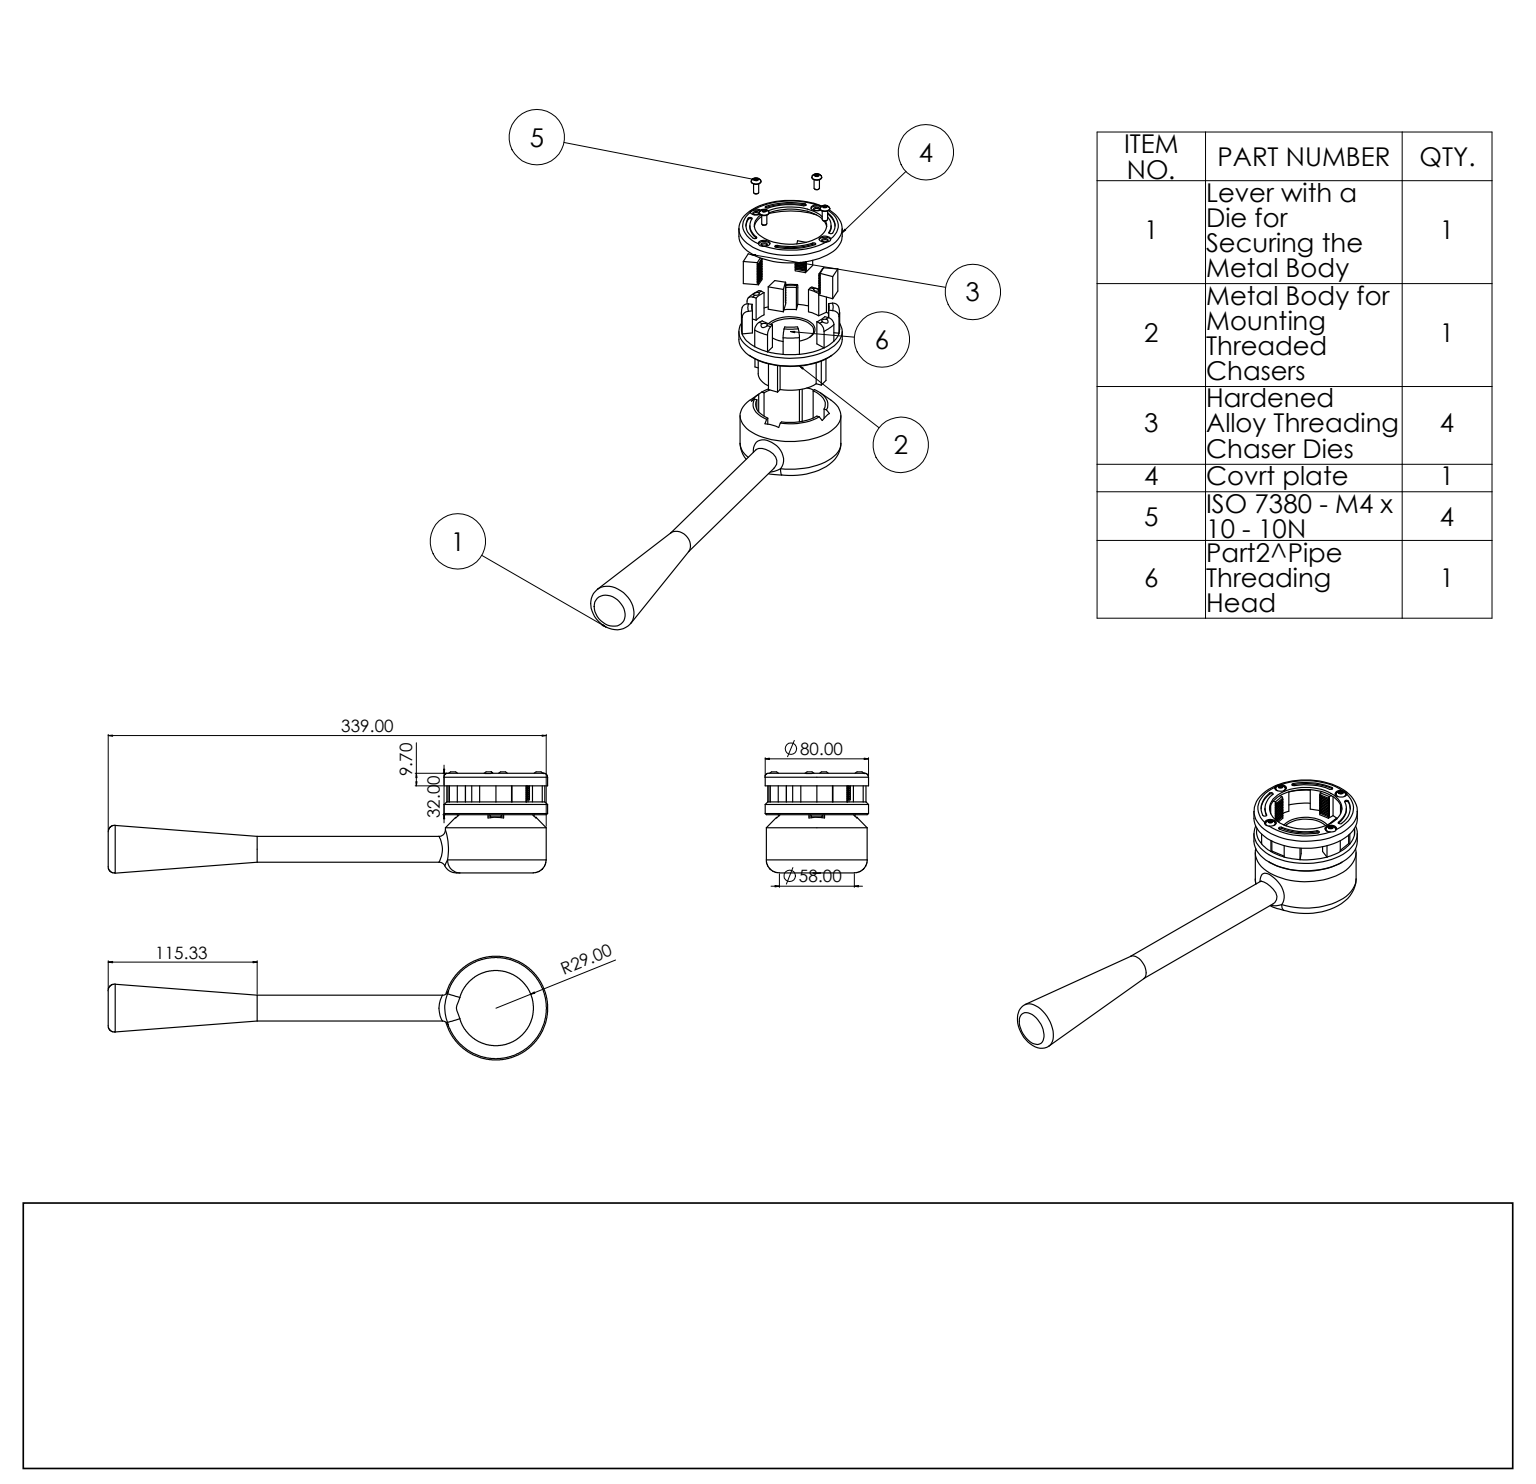
ISO-10303-21;
HEADER;
FILE_DESCRIPTION (('STEP AP214'),
    '1' );
FILE_NAME ('MAS-312',
    '2026-10-19T14:05:14',
    ( '' ),
    ( '' ),
    'SwSTEP 2.0',
    'SolidWorks 2025',
    '' );
FILE_SCHEMA (( 'AUTOMOTIVE_DESIGN' ));
ENDSEC;

DATA;
#1 = AXIS2_PLACEMENT_3D ( 'NONE', #3987, #6980, #243 ) ;
#2 = CARTESIAN_POINT ( 'NONE',  ( -12.48950176432141923, 54.99999999999999289, -35.88888888888889284 ) ) ;
#3 = ORIENTED_EDGE ( 'NONE', *, *, #1774, .T. ) ;
#4 = DIRECTION ( 'NONE',  ( 1.000000000000000000, 0.000000000000000000, -0.000000000000000000 ) ) ;
#5 = CARTESIAN_POINT ( 'NONE',  ( 3.853297297556091738, -8.887944228554063741, 39.26446342091823993 ) ) ;
#6 = ORIENTED_EDGE ( 'NONE', *, *, #748, .T. ) ;
#7 = DIRECTION ( 'NONE',  ( 0.000000000000000000, 0.000000000000000000, 1.000000000000000000 ) ) ;
#8 = LINE ( 'NONE', #7609, #8604 ) ;
#9 = ORIENTED_EDGE ( 'NONE', *, *, #8476, .T. ) ;
#10 = CARTESIAN_POINT ( 'NONE',  ( 11.49838106938660509, -4.251877780921969219, 37.26706069643609709 ) ) ;
#11 = ITEM_DEFINED_TRANSFORMATION ( 'NONE', 'NONE', #6463,  #6314 ) ;
#12 = ORIENTED_EDGE ( 'NONE', *, *, #8842, .T. ) ;
#13 = CARTESIAN_POINT ( 'NONE',  ( 6.000000000000007994, -10.00000000000000533, 31.00000000000000711 ) ) ;
#14 = CARTESIAN_POINT ( 'NONE',  ( 6.000000000000007994, 28.28385863652523824, 30.12488991936162108 ) ) ;
#15 = ORIENTED_EDGE ( 'NONE', *, *, #6125, .T. ) ;
#16 = CARTESIAN_POINT ( 'NONE',  ( 0.000000000000000000, 39.99999999999999289, 0.000000000000000000 ) ) ;
#17 = ORIENTED_EDGE ( 'NONE', *, *, #1471, .T. ) ;
#18 = CARTESIAN_POINT ( 'NONE',  ( 1.030449557444946671E-26, 53.50000000000031264, -26.00000000000004974 ) ) ;
#19 = DIRECTION ( 'NONE',  ( 0.000000000000000000, 0.000000000000000000, 1.000000000000000000 ) ) ;
#20 = CARTESIAN_POINT ( 'NONE',  ( -0.01963426291156584666, -6.705128248126137613, 43.99999014335539016 ) ) ;
#21 = MECHANICAL_DESIGN_GEOMETRIC_PRESENTATION_REPRESENTATION (  '', ( #1599 ), #7104 ) ;
#22 = VERTEX_POINT ( 'NONE', #2863 ) ;
#23 = CARTESIAN_POINT ( 'NONE',  ( -7.995545880304240960, 59.98659813632739457, 32.45264704635820152 ) ) ;
#24 = ORIENTED_EDGE ( 'NONE', *, *, #464, .F. ) ;
#25 = PRODUCT_DEFINITION_CONTEXT ( 'detailed design', #5808, 'design' ) ;
#26 = ORIENTED_EDGE ( 'NONE', *, *, #454, .F. ) ;
#28 = AXIS2_PLACEMENT_3D ( 'NONE', #4537, #730, #2939 ) ;
#27 = PLANE ( 'NONE',  #7404 ) ;
#29 = CARTESIAN_POINT ( 'NONE',  ( -0.01628753085184865904, -6.705134819200520901, 38.99999783451422530 ) ) ;
#30 = FACE_OUTER_BOUND ( 'NONE', #6374, .T. ) ;
#31 = DIRECTION ( 'NONE',  ( 0.000000000000000000, 0.000000000000000000, 1.000000000000000000 ) ) ;
#32 = ORIENTED_EDGE ( 'NONE', *, *, #3378, .T. ) ;
#33 = CARTESIAN_POINT ( 'NONE',  ( 28.34870838944214100, 59.99999999999999289, 9.815840903884559765 ) ) ;
#34 = ADVANCED_FACE ( 'NONE', ( #5878 ), #8015, .T. ) ;
#35 = EDGE_CURVE ( 'NONE', #8414, #7328, #2773, .T. ) ;
#36 = ORIENTED_EDGE ( 'NONE', *, *, #1808, .T. ) ;
#37 = CARTESIAN_POINT ( 'NONE',  ( -7.819489076939736272, 61.89591950820473443, 36.97167050927867393 ) ) ;
#38 = CARTESIAN_POINT ( 'NONE',  ( 1.084683744678891232E-26, 59.63872771225970837, -25.64778813235487220 ) ) ;
#39 = VECTOR ( 'NONE', #8891, 1000.000000000000000 ) ;
#40 = CARTESIAN_POINT ( 'NONE',  ( -8.673617379884032514E-16, 30.00000000000000000, -4.000000000000002665 ) ) ;
#41 = EDGE_CURVE ( 'NONE', #3849, #2645, #7411, .T. ) ;
#42 = CARTESIAN_POINT ( 'NONE',  ( 1.300000000000000044, -0.7216878364870317197, -1.250000000000000000 ) ) ;
#43 = CYLINDRICAL_SURFACE ( 'NONE', #4602, 1.999999999999999556 ) ;
#44 = DIRECTION ( 'NONE',  ( -1.000000000000000000, 0.000000000000000000, 0.000000000000000000 ) ) ;
#45 = ORIENTED_EDGE ( 'NONE', *, *, #2688, .T. ) ;
#46 = DIRECTION ( 'NONE',  ( -0.000000000000000000, 0.000000000000000000, 1.000000000000000000 ) ) ;
#47 = VECTOR ( 'NONE', #1280, 1000.000000000000000 ) ;
#48 = ADVANCED_FACE ( 'NONE', ( #1481 ), #9105, .T. ) ;
#49 = VERTEX_POINT ( 'NONE', #7520 ) ;
#50 = DIRECTION ( 'NONE',  ( 0.000000000000000000, 0.000000000000000000, 1.000000000000000000 ) ) ;
#51 = EDGE_CURVE ( 'NONE', #326, #7682, #6952, .T. ) ;
#52 = ORIENTED_EDGE ( 'NONE', *, *, #3525, .F. ) ;
#53 = CARTESIAN_POINT ( 'NONE',  ( 38.00000000000000711, 59.99999999999999289, 1.288922537256478387E-13 ) ) ;
#54 = CARTESIAN_POINT ( 'NONE',  ( 4.579605370182076030, -8.646111723837565322, 39.15306555959272572 ) ) ;
#55 = CIRCLE ( 'NONE', #3026, 27.00000000000000355 ) ;
#56 = CIRCLE ( 'NONE', #3832, 38.00000000000000711 ) ;
#57 = EDGE_LOOP ( 'NONE', ( #2932, #7865, #7571, #5966, #8095 ) ) ;
#58 = DIRECTION ( 'NONE',  ( 0.000000000000000000, 1.000000000000000000, 0.000000000000000000 ) ) ;
#59 = DIRECTION ( 'NONE',  ( -1.000000000000000000, 0.000000000000000000, 1.084202172485503448E-16 ) ) ;
#60 = ORIENTED_EDGE ( 'NONE', *, *, #1877, .F. ) ;
#61 = AXIS2_PLACEMENT_3D ( 'NONE', #6025, #2270, #8317 ) ;
#62 = CARTESIAN_POINT ( 'NONE',  ( 10.00081333311621989, 3.643253863043277363, 37.85858479645732899 ) ) ;
#63 = PRODUCT_CONTEXT ( 'NONE', #3923, 'mechanical' ) ;
#64 = VERTEX_POINT ( 'NONE', #213 ) ;
#65 = EDGE_LOOP ( 'NONE', ( #1698, #9286, #7170, #5423 ) ) ;
#66 = LINE ( 'NONE', #799, #8451 ) ;
#67 = CARTESIAN_POINT ( 'NONE',  ( -26.32489316217636954, -15.00000000000000000, 6.000000000000009770 ) ) ;
#68 = CARTESIAN_POINT ( 'NONE',  ( -3.999999999999999112, 28.99999999999997158, 24.67792535850613334 ) ) ;
#69 = ORIENTED_EDGE ( 'NONE', *, *, #3277, .T. ) ;
#70 = CARTESIAN_POINT ( 'NONE',  ( 0.000000000000000000, 0.000000000000000000, 0.000000000000000000 ) ) ;
#71 = VERTEX_POINT ( 'NONE', #9199 ) ;
#72 = CARTESIAN_POINT ( 'NONE',  ( -9.983292374582678264, 3.962892183205132479, 41.37334990339741125 ) ) ;
#73 = DIRECTION ( 'NONE',  ( 0.000000000000000000, 1.000000000000000000, 0.000000000000000000 ) ) ;
#74 = EDGE_CURVE ( 'NONE', #2204, #4788, #7083, .T. ) ;
#75 = DIRECTION ( 'NONE',  ( -1.735493991486225972E-29, 6.508102468073347395E-30, 1.000000000000000000 ) ) ;
#76 = AXIS2_PLACEMENT_3D ( 'NONE', #8734, #591, #7241 ) ;
#77 = VERTEX_POINT ( 'NONE', #3810 ) ;
#78 = CARTESIAN_POINT ( 'NONE',  ( 28.33333333333337478, 39.99999999999999289, -9.860132971832594961 ) ) ;
#79 = CARTESIAN_POINT ( 'NONE',  ( 20.99999999999999645, 30.00000000000000000, 4.000000000000000888 ) ) ;
#80 = ORIENTED_EDGE ( 'NONE', *, *, #3650, .T. ) ;
#81 = EDGE_LOOP ( 'NONE', ( #9222, #5342, #9321, #2491 ) ) ;
#82 = CARTESIAN_POINT ( 'NONE',  ( -2.771370799027269349, -6.331017003992445602, 38.93346330084214202 ) ) ;
#83 = CARTESIAN_POINT ( 'NONE',  ( 0.000000000000000000, 0.000000000000000000, 0.000000000000000000 ) ) ;
#84 = AXIS2_PLACEMENT_3D ( 'NONE', #4346, #782, #3690 ) ;
#85 = AXIS2_PLACEMENT_3D ( 'NONE', #944, #4059, #1772 ) ;
#86 = DIRECTION ( 'NONE',  ( 0.000000000000000000, 0.000000000000000000, 1.000000000000000000 ) ) ;
#87 = PRODUCT_DEFINITION_SHAPE ( 'NONE', 'NONE',  #9761 ) ;
#88 = ORIENTED_EDGE ( 'NONE', *, *, #8502, .F. ) ;
#89 = CARTESIAN_POINT ( 'NONE',  ( 5.562309845534588959, 60.99999999999999289, -30.56426808735054479 ) ) ;
#90 = AXIS2_PLACEMENT_3D ( 'NONE', #5171, #7481, #672 ) ;
#91 = ORIENTED_EDGE ( 'NONE', *, *, #7636, .T. ) ;
#92 = CARTESIAN_POINT ( 'NONE',  ( 5.562309845534588959, 49.99999999999999289, -33.06426808735054124 ) ) ;
#93 = EDGE_CURVE ( 'NONE', #9341, #7266, #8353, .T. ) ;
#94 = DIRECTION ( 'NONE',  ( -0.000000000000000000, -0.5000000000000001110, -0.8660254037844385966 ) ) ;
#95 = CARTESIAN_POINT ( 'NONE',  ( 24.67792535850613334, 0.000000000000000000, 4.000000000000000888 ) ) ;
#96 = CARTESIAN_POINT ( 'NONE',  ( 0.000000000000000000, 0.000000000000000000, 0.000000000000000000 ) ) ;
#97 = CARTESIAN_POINT ( 'NONE',  ( -6.850714361783683870, -15.00000000000000000, 28.25199985127544977 ) ) ;
#98 = CARTESIAN_POINT ( 'NONE',  ( -34.07933880998930221, 60.99999999999999289, 5.371095444502539173 ) ) ;
#99 = DIRECTION ( 'NONE',  ( 0.9449569463147374782, 0.000000000000000000, 0.3271946967961527619 ) ) ;
#100 = ORIENTED_EDGE ( 'NONE', *, *, #2687, .F. ) ;
#101 = DIRECTION ( 'NONE',  ( 0.000000000000000000, -1.000000000000000000, 0.000000000000000000 ) ) ;
#102 = VECTOR ( 'NONE', #2807, 1000.000000000000000 ) ;
#103 = VECTOR ( 'NONE', #6274, 1000.000000000000341 ) ;
#104 = CIRCLE ( 'NONE', #7815, 26.00000000000012790 ) ;
#105 = AXIS2_PLACEMENT_3D ( 'NONE', #139, #1748, #4771 ) ;
#106 = EDGE_CURVE ( 'NONE', #1933, #8061, #806, .T. ) ;
#107 = EDGE_CURVE ( 'NONE', #2537, #9428, #3759, .T. ) ;
#108 = VECTOR ( 'NONE', #4796, 1000.000000000000000 ) ;
#109 = AXIS2_PLACEMENT_3D ( 'NONE', #9198, #4705, #305 ) ;
#110 = CARTESIAN_POINT ( 'NONE',  ( 8.948640893600852668E-27, 42.50000000000020606, -25.00000000000000000 ) ) ;
#111 = ORIENTED_EDGE ( 'NONE', *, *, #684, .T. ) ;
#112 = DIRECTION ( 'NONE',  ( 0.000000000000000000, -1.000000000000000000, 0.000000000000000000 ) ) ;
#113 = CARTESIAN_POINT ( 'NONE',  ( 2.825938509006990174, -14.99999999999936762, 36.77312956257851084 ) ) ;
#114 = ORIENTED_EDGE ( 'NONE', *, *, #8852, .F. ) ;
#115 = ADVANCED_FACE ( 'NONE', ( #5243 ), #6016, .F. ) ;
#116 = DIRECTION ( 'NONE',  ( -0.000000000000000000, -1.000000000000000000, -0.000000000000000000 ) ) ;
#117 = AXIS2_PLACEMENT_3D ( 'NONE', #7294, #7143, #4982 ) ;
#118 = ADVANCED_FACE ( 'NONE', ( #1539 ), #6120, .T. ) ;
#119 = CARTESIAN_POINT ( 'NONE',  ( -8.216777476527294510, 42.50000000000020606, -23.61111111111107519 ) ) ;
#120 = CLOSED_SHELL ( 'NONE', ( #1419, #7952, #2099, #3958, #3679, #8907, #3700, #3725, #1256, #288, #9736, #7646, #7332, #6776, #8180, #48, #7507, #2171, #4864, #7401, #2702, #2733, #7456, #636, #936, #1118, #6024, #1058, #540, #1404, #1588, #7209, #115, #1059, #588, #939, #8009, #6508, #1237, #2007, #4157, #6912, #2948, #702, #4090, #7822, #4876, #3409, #2741, #2560, #1004, #4751, #8856, #1093, #818, #5216, #1926, #9214, #9112, #7707, #4600, #634, #1660, #1234, #9684, #1433, #2142, #7068, #5305, #2300, #8588, #5110, #8978, #5514, #6739, #8244, #7533, #7708, #9094, #6502, #6348, #7871, #6449, #6840, #9282, #4029, #5531, #4774, #891, #5599, #3099, #5594, #5412, #1186, #7274, #6763, #3544, #3838, #1663, #3596, #7633, #5416, #9580, #6826, #5045, #4533, #1363 ) ) ;
#121 = ORIENTED_EDGE ( 'NONE', *, *, #2139, .T. ) ;
#122 = CARTESIAN_POINT ( 'NONE',  ( 8.958048712684526294, -1.161593745032227565, 41.89873932196367434 ) ) ;
#123 = ORIENTED_EDGE ( 'NONE', *, *, #454, .T. ) ;
#124 = DIRECTION ( 'NONE',  ( 0.000000000000000000, 0.000000000000000000, 1.000000000000000000 ) ) ;
#125 = CIRCLE ( 'NONE', #905, 26.00000000000000355 ) ;
#126 = CARTESIAN_POINT ( 'NONE',  ( -28.87459861216645862, 60.99999999999999289, -14.47678174684361352 ) ) ;
#127 = LINE ( 'NONE', #9051, #3388 ) ;
#128 = ORIENTED_EDGE ( 'NONE', *, *, #8520, .F. ) ;
#129 = LINE ( 'NONE', #4464, #7033 ) ;
#130 = ORIENTED_EDGE ( 'NONE', *, *, #5654, .T. ) ;
#131 = CARTESIAN_POINT ( 'NONE',  ( -7.290079979600610827, 10.14749281417268811, 42.62097616879101025 ) ) ;
#132 = CARTESIAN_POINT ( 'NONE',  ( 4.000000000000001776, 28.99999999999997158, -24.67792535850613334 ) ) ;
#133 = CARTESIAN_POINT ( 'NONE',  ( -5.562309845534701758, 60.99999999999999289, 33.06426808735052703 ) ) ;
#134 = ORIENTED_EDGE ( 'NONE', *, *, #5755, .F. ) ;
#135 = DIRECTION ( 'NONE',  ( -0.000000000000000000, -1.000000000000000000, -0.000000000000000000 ) ) ;
#136 = ORIENTED_EDGE ( 'NONE', *, *, #3165, .T. ) ;
#137 = VERTEX_POINT ( 'NONE', #6145 ) ;
#138 = FACE_OUTER_BOUND ( 'NONE', #6010, .T. ) ;
#139 = CARTESIAN_POINT ( 'NONE',  ( 0.000000000000000000, 54.99999999999999289, 0.000000000000000000 ) ) ;
#140 = CARTESIAN_POINT ( 'NONE',  ( 32.85680095556730862, 59.99999999999999289, 3.070933240276029874 ) ) ;
#141 = ORIENTED_EDGE ( 'NONE', *, *, #4576, .F. ) ;
#142 = DIRECTION ( 'NONE',  ( -0.000000000000000000, -1.000000000000000000, -0.000000000000000000 ) ) ;
#143 = ORIENTED_EDGE ( 'NONE', *, *, #5654, .F. ) ;
#144 = FACE_OUTER_BOUND ( 'NONE', #5084, .T. ) ;
#145 = LINE ( 'NONE', #38, #7530 ) ;
#146 = LINE ( 'NONE', #3335, #665 ) ;
#147 =( LENGTH_UNIT ( ) NAMED_UNIT ( * ) SI_UNIT ( .MILLI., .METRE. ) );
#148 = DIRECTION ( 'NONE',  ( 0.000000000000000000, 0.000000000000000000, -1.000000000000000000 ) ) ;
#149 = FACE_OUTER_BOUND ( 'NONE', #9484, .T. ) ;
#150 = ADVANCED_FACE ( 'NONE', ( #6740 ), #686, .F. ) ;
#151 = CARTESIAN_POINT ( 'NONE',  ( 4.000000000000007994, 30.00000000000000000, 24.67792535850613334 ) ) ;
#152 = CARTESIAN_POINT ( 'NONE',  ( 5.562309845534588959, 59.99999999999999289, -30.56426808735054479 ) ) ;
#153 = ORIENTED_EDGE ( 'NONE', *, *, #7147, .T. ) ;
#154 = DIRECTION ( 'NONE',  ( 0.9860132971832693549, 1.788557213313974126E-28, -0.1666666666666657970 ) ) ;
#155 = CARTESIAN_POINT ( 'NONE',  ( 37.34143203299149860, 61.94837758590841759, 4.137096292553819055 ) ) ;
#156 = VERTEX_POINT ( 'NONE', #6690 ) ;
#157 = CYLINDRICAL_SURFACE ( 'NONE', #6340, 39.00000000000002132 ) ;
#158 = CARTESIAN_POINT ( 'NONE',  ( -8.216777476527294510, 50.00000000000032685, -23.61111111111111427 ) ) ;
#159 = ORIENTED_EDGE ( 'NONE', *, *, #5056, .F. ) ;
#160 = AXIS2_PLACEMENT_3D ( 'NONE', #5562, #8483, #3937 ) ;
#161 = CARTESIAN_POINT ( 'NONE',  ( 1.729137406965966184, -11.61013223293034713, 38.97104407561932504 ) ) ;
#162 = DIRECTION ( 'NONE',  ( 0.000000000000000000, 0.000000000000000000, 1.000000000000000000 ) ) ;
#163 = EDGE_CURVE ( 'NONE', #7794, #4048, #3844, .T. ) ;
#164 = ADVANCED_FACE ( 'NONE', ( #5228 ), #5133, .F. ) ;
#165 = CARTESIAN_POINT ( 'NONE',  ( -4.331874290630486790, 29.33187429063046991, 24.96033808169876878 ) ) ;
#166 = EDGE_CURVE ( 'NONE', #996, #8756, #7398, .T. ) ;
#167 = VERTEX_POINT ( 'NONE', #7496 ) ;
#168 = FACE_OUTER_BOUND ( 'NONE', #440, .T. ) ;
#169 = EDGE_CURVE ( 'NONE', #2001, #9443, #8039, .T. ) ;
#170 = ORIENTED_EDGE ( 'NONE', *, *, #4564, .F. ) ;
#171 = VECTOR ( 'NONE', #8479, 1000.000000000000000 ) ;
#172 = CIRCLE ( 'NONE', #6452, 38.00000000000000711 ) ;
#173 = PRODUCT_DEFINITION_SHAPE ( 'NONE', 'NONE',  #9757 ) ;
#174 = CARTESIAN_POINT ( 'NONE',  ( 4.000000000000002665, 30.00000000000000000, -8.673617379884032514E-16 ) ) ;
#175 = FACE_OUTER_BOUND ( 'NONE', #2105, .T. ) ;
#176 = VECTOR ( 'NONE', #6148, 1000.000000000000000 ) ;
#177 = ORIENTED_EDGE ( 'NONE', *, *, #6292, .F. ) ;
#178 = CARTESIAN_POINT ( 'NONE',  ( -7.935670091272695181, 60.00000000000000711, 32.24976038726180860 ) ) ;
#179 = VERTEX_POINT ( 'NONE', #3191 ) ;
#180 = ORIENTED_EDGE ( 'NONE', *, *, #6176, .F. ) ;
#181 = CARTESIAN_POINT ( 'NONE',  ( -3.564217818894435563, -6.054132172044422333, 43.67637224480981217 ) ) ;
#182 = DIRECTION ( 'NONE',  ( 0.000000000000000000, 0.000000000000000000, -1.000000000000000000 ) ) ;
#183 = CIRCLE ( 'NONE', #5688, 37.99999999999999289 ) ;
#184 = CARTESIAN_POINT ( 'NONE',  ( 31.11591804390324612, 60.99999999999999289, -4.904043666719942074 ) ) ;
#185 = VERTEX_POINT ( 'NONE', #9279 ) ;
#186 = CARTESIAN_POINT ( 'NONE',  ( -29.00000000000000355, 30.00000000000000000, 4.000000000000010658 ) ) ;
#187 = LINE ( 'NONE', #9125, #4256 ) ;
#188 =( GEOMETRIC_REPRESENTATION_CONTEXT ( 3 ) GLOBAL_UNCERTAINTY_ASSIGNED_CONTEXT ( ( #1496 ) ) GLOBAL_UNIT_ASSIGNED_CONTEXT ( ( #3676, #5943, #2174 ) ) REPRESENTATION_CONTEXT ( 'NONE', 'WORKASPACE' ) );
#189 = ORIENTED_EDGE ( 'NONE', *, *, #8556, .F. ) ;
#190 = DIRECTION ( 'NONE',  ( 0.000000000000000000, -0.000000000000000000, 1.000000000000000000 ) ) ;
#191 = CARTESIAN_POINT ( 'NONE',  ( 7.856683717344210116, 59.59863544270934455, -34.07748394475226661 ) ) ;
#192 = LINE ( 'NONE', #2440, #6007 ) ;
#193 = CARTESIAN_POINT ( 'NONE',  ( 5.031243191487485333, 17.19748707720165370, 38.67840086860066151 ) ) ;
#194 = CARTESIAN_POINT ( 'NONE',  ( 0.000000000000000000, 54.99999999999999289, 0.000000000000000000 ) ) ;
#195 = ORIENTED_EDGE ( 'NONE', *, *, #1181, .F. ) ;
#196 = CARTESIAN_POINT ( 'NONE',  ( 12.43339847825378364, 39.99999999999999289, -35.90836395996003461 ) ) ;
#197 = EDGE_CURVE ( 'NONE', #4918, #1409, #1885, .T. ) ;
#198 = CIRCLE ( 'NONE', #6955, 4.500000000000005329 ) ;
#199 = DIRECTION ( 'NONE',  ( 0.000000000000000000, 0.000000000000000000, 1.000000000000000000 ) ) ;
#200 = DIRECTION ( 'NONE',  ( 0.000000000000000000, 0.000000000000000000, 1.000000000000000000 ) ) ;
#201 = EDGE_CURVE ( 'NONE', #5205, #8953, #1759, .T. ) ;
#202 = ORIENTED_EDGE ( 'NONE', *, *, #8489, .F. ) ;
#203 = DIRECTION ( 'NONE',  ( 0.000000000000000000, 0.000000000000000000, 1.000000000000000000 ) ) ;
#204 = CARTESIAN_POINT ( 'NONE',  ( 33.06426808735054124, 59.99576382555915899, 3.062309845534584074 ) ) ;
#205 = ORIENTED_EDGE ( 'NONE', *, *, #694, .T. ) ;
#206 = AXIS2_PLACEMENT_3D ( 'NONE', #7812, #2466, #1194 ) ;
#207 = CARTESIAN_POINT ( 'NONE',  ( 0.000000000000000000, 30.00000000000000000, 0.000000000000000000 ) ) ;
#208 = DIRECTION ( 'NONE',  ( 0.000000000000000000, -1.000000000000000000, 0.000000000000000000 ) ) ;
#209 = VERTEX_POINT ( 'NONE', #7698 ) ;
#210 = CARTESIAN_POINT ( 'NONE',  ( 12.20000000000000107, 0.000000000000000000, 0.000000000000000000 ) ) ;
#211 = AXIS2_PLACEMENT_3D ( 'NONE', #6008, #116, #5285 ) ;
#212 = DIRECTION ( 'NONE',  ( 0.000000000000000000, 0.000000000000000000, 1.000000000000000000 ) ) ;
#213 = CARTESIAN_POINT ( 'NONE',  ( 4.653657836759942730E-15, 52.29648987751954792, 38.00000000000000711 ) ) ;
#214 = CARTESIAN_POINT ( 'NONE',  ( 8.948640893600852668E-27, 42.50000000000020606, -25.00000000000000000 ) ) ;
#215 = ORIENTED_EDGE ( 'NONE', *, *, #2320, .T. ) ;
#216 = CARTESIAN_POINT ( 'NONE',  ( 3.429011037612588487E-15, 0.000000000000000000, 27.99999999999999289 ) ) ;
#217 = ADVANCED_FACE ( 'NONE', ( #8822 ), #7238, .F. ) ;
#218 = ORIENTED_EDGE ( 'NONE', *, *, #4973, .T. ) ;
#219 = CARTESIAN_POINT ( 'NONE',  ( 33.06426808735054124, 49.99999999999999289, 5.562309845534586294 ) ) ;
#220 = AXIS2_PLACEMENT_3D ( 'NONE', #9694, #2922, #5107 ) ;
#221 = CARTESIAN_POINT ( 'NONE',  ( 0.000000000000000000, 30.00000000000000000, 0.000000000000000000 ) ) ;
#222 = CIRCLE ( 'NONE', #6654, 1.500000000000000888 ) ;
#223 = EDGE_CURVE ( 'NONE', #5194, #1935, #3139, .T. ) ;
#224 = EDGE_CURVE ( 'NONE', #6202, #6468, #9617, .T. ) ;
#225 = CIRCLE ( 'NONE', #5729, 4.500000000000005329 ) ;
#226 = EDGE_CURVE ( 'NONE', #987, #5419, #6349, .T. ) ;
#227 = ORIENTED_EDGE ( 'NONE', *, *, #8008, .F. ) ;
#228 = CARTESIAN_POINT ( 'NONE',  ( -33.72085295419949347, 59.72647237447257851, -7.995677060003914427 ) ) ;
#229 = ORIENTED_EDGE ( 'NONE', *, *, #4215, .T. ) ;
#230 = ORIENTED_EDGE ( 'NONE', *, *, #1372, .F. ) ;
#231 = ORIENTED_EDGE ( 'NONE', *, *, #8364, .T. ) ;
#232 = CARTESIAN_POINT ( 'NONE',  ( -8.545448575588375562, 56.00000000000030553, -24.55555555555558911 ) ) ;
#233 = SURFACE_SIDE_STYLE ('',( #8473 ) ) ;
#234 = FACE_OUTER_BOUND ( 'NONE', #8971, .T. ) ;
#235 = EDGE_CURVE ( 'NONE', #6362, #4125, #4927, .T. ) ;
#236 = ORIENTED_EDGE ( 'NONE', *, *, #3146, .F. ) ;
#237 = EDGE_CURVE ( 'NONE', #1437, #3718, #3681, .T. ) ;
#238 = ORIENTED_EDGE ( 'NONE', *, *, #9403, .F. ) ;
#239 = DIRECTION ( 'NONE',  ( 0.000000000000000000, 1.000000000000000000, 0.000000000000000000 ) ) ;
#240 = ORIENTED_EDGE ( 'NONE', *, *, #7837, .T. ) ;
#241 = CARTESIAN_POINT ( 'NONE',  ( 0.000000000000000000, 60.99999999999999289, 0.000000000000000000 ) ) ;
#242 = DIRECTION ( 'NONE',  ( 0.000000000000000000, 0.000000000000000000, -1.000000000000000000 ) ) ;
#243 = DIRECTION ( 'NONE',  ( 0.000000000000000000, 0.000000000000000000, 1.000000000000000000 ) ) ;
#244 = AXIS2_PLACEMENT_3D ( 'NONE', #7628, #7725, #2222 ) ;
#245 = AXIS2_PLACEMENT_3D ( 'NONE', #2886, #4538, #6229 ) ;
#246 = CYLINDRICAL_SURFACE ( 'NONE', #7429, 1.500000000000001332 ) ;
#247 = ORIENTED_EDGE ( 'NONE', *, *, #9110, .F. ) ;
#248 = LINE ( 'NONE', #2485, #2906 ) ;
#249 = EDGE_CURVE ( 'NONE', #5097, #3498, #5520, .T. ) ;
#250 = AXIS2_PLACEMENT_3D ( 'NONE', #2833, #9708, #7388 ) ;
#251 = DIRECTION ( 'NONE',  ( 0.000000000000000000, 1.000000000000000000, 0.000000000000000000 ) ) ;
#252 = VERTEX_POINT ( 'NONE', #7632 ) ;
#253 = FACE_OUTER_BOUND ( 'NONE', #1428, .T. ) ;
#254 = CARTESIAN_POINT ( 'NONE',  ( 1.820000000000000062, 0.000000000000000000, 0.000000000000000000 ) ) ;
#255 = EDGE_CURVE ( 'NONE', #1637, #4569, #2387, .T. ) ;
#256 = ORIENTED_EDGE ( 'NONE', *, *, #2384, .T. ) ;
#257 = CIRCLE ( 'NONE', #6534, 9.999999999999998224 ) ;
#258 = CIRCLE ( 'NONE', #2286, 27.99999999999999289 ) ;
#259 = CARTESIAN_POINT ( 'NONE',  ( -15.97678174684350871, 60.99999999999999289, 30.37459861216651191 ) ) ;
#260 = DIRECTION ( 'NONE',  ( -1.735493991486225972E-29, 6.508102468073347395E-30, 1.000000000000000000 ) ) ;
#261 = VECTOR ( 'NONE', #1095, 1000.000000000000114 ) ;
#262 = VECTOR ( 'NONE', #9116, 1000.000000000000114 ) ;
#263 = LINE ( 'NONE', #7803, #7090 ) ;
#264 = VECTOR ( 'NONE', #8760, 1000.000000000000000 ) ;
#265 = CARTESIAN_POINT ( 'NONE',  ( -8.216777476527294510, 56.50000000000029843, -23.61111111111111427 ) ) ;
#266 = ORIENTED_EDGE ( 'NONE', *, *, #8114, .T. ) ;
#267 = CARTESIAN_POINT ( 'NONE',  ( 0.000000000000000000, 37.99999999999996447, -40.00000000000000711 ) ) ;
#268 = PLANE ( 'NONE',  #1365 ) ;
#269 = VERTEX_POINT ( 'NONE', #3889 ) ;
#270 = AXIS2_PLACEMENT_3D ( 'NONE', #2075, #7132, #3665 ) ;
#271 = CARTESIAN_POINT ( 'NONE',  ( 29.24912810952613640, 29.14236109046821710, 6.000000000000000000 ) ) ;
#272 = CARTESIAN_POINT ( 'NONE',  ( -28.87459861216645862, 60.99999999999999289, -15.97678174684361707 ) ) ;
#273 = EDGE_CURVE ( 'NONE', #4125, #4231, #5470, .T. ) ;
#274 = VECTOR ( 'NONE', #1912, 1000.000000000000341 ) ;
#275 = ORIENTED_EDGE ( 'NONE', *, *, #6897, .F. ) ;
#276 = CARTESIAN_POINT ( 'NONE',  ( -35.47893788052810038, 58.98370868798952671, -6.231324730575372506 ) ) ;
#277 = ORIENTED_EDGE ( 'NONE', *, *, #1811, .F. ) ;
#278 = DIRECTION ( 'NONE',  ( 0.000000000000000000, 0.000000000000000000, 1.000000000000000000 ) ) ;
#279 = VERTEX_POINT ( 'NONE', #6422 ) ;
#280 = EDGE_CURVE ( 'NONE', #8145, #2204, #7893, .T. ) ;
#281 = ORIENTED_EDGE ( 'NONE', *, *, #7582, .F. ) ;
#282 = CARTESIAN_POINT ( 'NONE',  ( -9.999399707319170716, 3.681889571620033497, 37.85894501931166900 ) ) ;
#283 = LINE ( 'NONE', #3269, #6859 ) ;
#284 = CARTESIAN_POINT ( 'NONE',  ( 9.318419442923201951E-27, 47.00000000000034106, -25.00000000000000000 ) ) ;
#285 = VERTEX_POINT ( 'NONE', #824 ) ;
#286 = ORIENTED_EDGE ( 'NONE', *, *, #2067, .T. ) ;
#287 = CARTESIAN_POINT ( 'NONE',  ( 3.060768115627997776, 59.99034304420147379, -33.21665709534246957 ) ) ;
#288 = ADVANCED_FACE ( 'NONE', ( #6098 ), #6191, .T. ) ;
#289 = PLANE ( 'NONE',  #8040 ) ;
#290 = EDGE_CURVE ( 'NONE', #22, #2244, #187, .T. ) ;
#291 = CARTESIAN_POINT ( 'NONE',  ( 33.00000000000000711, 59.99999999999999289, 1.152188841818234386E-13 ) ) ;
#292 = ADVANCED_FACE ( 'NONE', ( #3127 ), #3178, .T. ) ;
#293 = DIRECTION ( 'NONE',  ( -0.000000000000000000, -1.000000000000000000, -0.000000000000000000 ) ) ;
#294 = VERTEX_POINT ( 'NONE', #8424 ) ;
#295 = CARTESIAN_POINT ( 'NONE',  ( -2.653525817520781855E-13, 39.99999999999999289, 38.00000000000000711 ) ) ;
#296 = ADVANCED_FACE ( 'NONE', ( #9221, #2433 ), #6373, .T. ) ;
#297 = ORIENTED_EDGE ( 'NONE', *, *, #6768, .F. ) ;
#298 = CARTESIAN_POINT ( 'NONE',  ( 5.137569555611264605, 61.99999999999999289, 32.59762842694627949 ) ) ;
#299 = DIRECTION ( 'NONE',  ( -0.000000000000000000, 1.000000000000000000, -0.000000000000000000 ) ) ;
#300 = VERTEX_POINT ( 'NONE', #423 ) ;
#301 = CARTESIAN_POINT ( 'NONE',  ( -5.022008081159694548, 11.94856982034775683, 43.35258044418206680 ) ) ;
#302 = CARTESIAN_POINT ( 'NONE',  ( 9.762153702110021092E-27, 45.50000000000019185, -25.00000000000000000 ) ) ;
#303 = CARTESIAN_POINT ( 'NONE',  ( 0.000000000000000000, 28.99999999999997158, 0.000000000000000000 ) ) ;
#304 = DIRECTION ( 'NONE',  ( -0.000000000000000000, 1.000000000000000000, 0.000000000000000000 ) ) ;
#305 = DIRECTION ( 'NONE',  ( 0.000000000000000000, 0.000000000000000000, 1.000000000000000000 ) ) ;
#306 = ORIENTED_EDGE ( 'NONE', *, *, #6531, .F. ) ;
#307 = LINE ( 'NONE', #9387, #9703 ) ;
#308 = ORIENTED_EDGE ( 'NONE', *, *, #4770, .F. ) ;
#309 = CARTESIAN_POINT ( 'NONE',  ( 9.219811829770575476E-27, 48.50000000000033396, -26.00000000000011369 ) ) ;
#310 = ORIENTED_EDGE ( 'NONE', *, *, #635, .T. ) ;
#311 = VECTOR ( 'NONE', #5751, 1000.000000000000000 ) ;
#312 = DIRECTION ( 'NONE',  ( 0.000000000000000000, 1.000000000000000000, 0.000000000000000000 ) ) ;
#313 = CARTESIAN_POINT ( 'NONE',  ( -5.562309845534584518, 49.99999999999999289, 35.56426808735054834 ) ) ;
#314 = ORIENTED_EDGE ( 'NONE', *, *, #2672, .F. ) ;
#315 = CARTESIAN_POINT ( 'NONE',  ( 33.06426808735054124, 60.99999999999999289, 5.562309845534586294 ) ) ;
#316 = ORIENTED_EDGE ( 'NONE', *, *, #2562, .T. ) ;
#317 = CARTESIAN_POINT ( 'NONE',  ( 0.000000000000000000, 1.000000000000014655, 0.000000000000000000 ) ) ;
#318 = ORIENTED_EDGE ( 'NONE', *, *, #9442, .F. ) ;
#319 = AXIS2_PLACEMENT_3D ( 'NONE', #6643, #8980, #9669 ) ;
#320 = CIRCLE ( 'NONE', #5041, 3.799999999999999378 ) ;
#321 = ORIENTED_EDGE ( 'NONE', *, *, #7835, .T. ) ;
#322 = CARTESIAN_POINT ( 'NONE',  ( -6.860056060574510894, -3.988295739037161614, 42.78128744368499525 ) ) ;
#323 = CARTESIAN_POINT ( 'NONE',  ( 23.54469556655648077, 59.99999999999999289, 29.82695610816123022 ) ) ;
#324 = CARTESIAN_POINT ( 'NONE',  ( 3.796404955196288922E-15, 27.99999999999992184, 31.00000000000000711 ) ) ;
#325 = CIRCLE ( 'NONE', #6298, 38.00000000000000711 ) ;
#326 = VERTEX_POINT ( 'NONE', #5646 ) ;
#327 = CARTESIAN_POINT ( 'NONE',  ( 2.326828918379978070E-15, 39.99999999999999289, -19.00000000000005684 ) ) ;
#328 = DIRECTION ( 'NONE',  ( 8.659560562354889717E-17, -0.7071067811865512365, 0.7071067811865439090 ) ) ;
#329 = CARTESIAN_POINT ( 'NONE',  ( 1.300000000000000044, -1.443375672974064328, -9.326206579303807412E-18 ) ) ;
#330 = DIRECTION ( 'NONE',  ( -0.9444444444444315412, 0.000000000000000000, 0.3286710990611268479 ) ) ;
#331 = CARTESIAN_POINT ( 'NONE',  ( 0.000000000000000000, 0.000000000000000000, 0.000000000000000000 ) ) ;
#332 = CARTESIAN_POINT ( 'NONE',  ( 0.000000000000000000, 30.00000000000000000, 0.000000000000000000 ) ) ;
#333 = AXIS2_PLACEMENT_3D ( 'NONE', #8336, #1619, #1570 ) ;
#334 = CARTESIAN_POINT ( 'NONE',  ( 33.06426808735054124, 49.99999999999999289, 3.062309845534584074 ) ) ;
#335 = EDGE_CURVE ( 'NONE', #2169, #1750, #9450, .T. ) ;
#336 = VECTOR ( 'NONE', #2888, 1000.000000000000000 ) ;
#337 = EDGE_CURVE ( 'NONE', #8698, #5898, #9303, .T. ) ;
#338 = EDGE_LOOP ( 'NONE', ( #2836, #3852, #9165, #3920 ) ) ;
#339 = CARTESIAN_POINT ( 'NONE',  ( -27.66666666666669272, 27.66666666666662167, 2.666666666666698049 ) ) ;
#340 = DIRECTION ( 'NONE',  ( 0.000000000000000000, 1.000000000000000000, 0.000000000000000000 ) ) ;
#341 = VERTEX_POINT ( 'NONE', #363 ) ;
#342 = DIRECTION ( 'NONE',  ( 0.000000000000000000, 0.000000000000000000, 1.000000000000000000 ) ) ;
#343 = CARTESIAN_POINT ( 'NONE',  ( 0.000000000000000000, 0.000000000000000000, -19.00000000000000355 ) ) ;
#344 = VERTEX_POINT ( 'NONE', #2620 ) ;
#345 = DIRECTION ( 'NONE',  ( -0.000000000000000000, -1.000000000000000000, -0.000000000000000000 ) ) ;
#346 = AXIS2_PLACEMENT_3D ( 'NONE', #4083, #2634, #9223 ) ;
#347 = AXIS2_PLACEMENT_3D ( 'NONE', #5096, #2713, #8750 ) ;
#348 = DIRECTION ( 'NONE',  ( 0.000000000000000000, 0.000000000000000000, 1.000000000000000000 ) ) ;
#349 = CARTESIAN_POINT ( 'NONE',  ( -37.45692540970868833, 61.81802411364413530, -6.576816292457711377 ) ) ;
#350 = EDGE_CURVE ( 'NONE', #3498, #6767, #2032, .T. ) ;
#351 = CARTESIAN_POINT ( 'NONE',  ( 0.5362474655584705818, -6.705996766429416667, 39.00014475790622726 ) ) ;
#352 = EDGE_CURVE ( 'NONE', #8330, #6149, #3299, .T. ) ;
#353 = CARTESIAN_POINT ( 'NONE',  ( 32.59762842694625817, 60.99999999999999289, -5.137569555611371186 ) ) ;
#354 = EDGE_LOOP ( 'NONE', ( #1511, #1589, #3120, #2364 ) ) ;
#355 = DIRECTION ( 'NONE',  ( 0.000000000000000000, 0.000000000000000000, 1.000000000000000000 ) ) ;
#356 = ORIENTED_EDGE ( 'NONE', *, *, #480, .F. ) ;
#357 = LINE ( 'NONE', #3258, #4214 ) ;
#358 = AXIS2_PLACEMENT_3D ( 'NONE', #6746, #9141, #8245 ) ;
#359 = EDGE_LOOP ( 'NONE', ( #7695, #5328, #4724, #356, #5569, #5542, #45, #4880, #4061 ) ) ;
#360 = LINE ( 'NONE', #5642, #2706 ) ;
#361 = CYLINDRICAL_SURFACE ( 'NONE', #4515, 2.500000000000002220 ) ;
#362 = CIRCLE ( 'NONE', #5560, 1.500000000000003109 ) ;
#363 = CARTESIAN_POINT ( 'NONE',  ( 5.562309845534588959, 60.99999999999999289, -35.56426808735054834 ) ) ;
#364 = ORIENTED_EDGE ( 'NONE', *, *, #965, .F. ) ;
#365 = CARTESIAN_POINT ( 'NONE',  ( 4.000000000000001776, 28.99999999999997158, -29.00000000000000355 ) ) ;
#366 = ORIENTED_EDGE ( 'NONE', *, *, #6545, .T. ) ;
#367 = ORIENTED_EDGE ( 'NONE', *, *, #5413, .T. ) ;
#368 = DIRECTION ( 'NONE',  ( 0.000000000000000000, 0.000000000000000000, -1.000000000000000000 ) ) ;
#369 = ORIENTED_EDGE ( 'NONE', *, *, #9442, .T. ) ;
#370 = ORIENTED_EDGE ( 'NONE', *, *, #6332, .F. ) ;
#371 = CARTESIAN_POINT ( 'NONE',  ( -9.589511961634933357, 6.242300754483544267, 37.96120689204327192 ) ) ;
#372 = CIRCLE ( 'NONE', #1158, 34.49999999999998579 ) ;
#373 = ADVANCED_FACE ( 'NONE', ( #4991, #2055, #5082, #4350, #4442, #6692 ), #1522, .T. ) ;
#374 = VECTOR ( 'NONE', #842, 1000.000000000000000 ) ;
#375 = CARTESIAN_POINT ( 'NONE',  ( 1.203012880462043003E-26, 59.00000000000029843, -25.00000000000000000 ) ) ;
#376 = CARTESIAN_POINT ( 'NONE',  ( -33.06426808735054124, 60.99999999999999289, -8.062309845534585406 ) ) ;
#377 = ORIENTED_EDGE ( 'NONE', *, *, #4261, .T. ) ;
#378 = CARTESIAN_POINT ( 'NONE',  ( 29.00000000000000355, 0.000000000000000000, 4.000000000000000000 ) ) ;
#379 = EDGE_LOOP ( 'NONE', ( #2512, #3295, #4858, #1225 ) ) ;
#380 = PLANE ( 'NONE',  #9644 ) ;
#381 = LINE ( 'NONE', #8854, #6240 ) ;
#382 = FACE_OUTER_BOUND ( 'NONE', #3255, .T. ) ;
#383 = FACE_OUTER_BOUND ( 'NONE', #9081, .T. ) ;
#384 = LINE ( 'NONE', #5665, #2838 ) ;
#385 = DIRECTION ( 'NONE',  ( 0.000000000000000000, -1.000000000000000000, 0.000000000000000000 ) ) ;
#386 = ADVANCED_FACE ( 'NONE', ( #5330 ), #2920, .T. ) ;
#387 = ORIENTED_EDGE ( 'NONE', *, *, #7583, .F. ) ;
#388 = VECTOR ( 'NONE', #3945, 1000.000000000000000 ) ;
#389 = CARTESIAN_POINT ( 'NONE',  ( 29.00000000000000355, 28.99999999999997158, 4.000000000000000000 ) ) ;
#390 = DIRECTION ( 'NONE',  ( -0.000000000000000000, 1.000000000000000000, 0.000000000000000000 ) ) ;
#391 = ORIENTED_EDGE ( 'NONE', *, *, #2229, .T. ) ;
#392 = CARTESIAN_POINT ( 'NONE',  ( 5.562309845534932684, 61.83753588906734677, -37.56426808735049150 ) ) ;
#393 = DIRECTION ( 'NONE',  ( 1.735493991486225972E-29, -6.508102468073347395E-30, -1.000000000000000000 ) ) ;
#394 = ORIENTED_EDGE ( 'NONE', *, *, #7055, .T. ) ;
#395 = PLANE ( 'NONE',  #2897 ) ;
#396 = EDGE_CURVE ( 'NONE', #1074, #9346, #9245, .T. ) ;
#397 = CARTESIAN_POINT ( 'NONE',  ( -9.860132971832692661, 59.99999999999999289, -28.33333333333334281 ) ) ;
#398 = AXIS2_PLACEMENT_3D ( 'NONE', #7354, #1376, #6045 ) ;
#399 = CIRCLE ( 'NONE', #2107, 2.199999999999999734 ) ;
#400 = CARTESIAN_POINT ( 'NONE',  ( -37.52916669695763119, 61.87792984901915361, -4.938418073206593206 ) ) ;
#401 = DIRECTION ( 'NONE',  ( 0.000000000000000000, 0.000000000000000000, -1.000000000000000000 ) ) ;
#402 = ORIENTED_EDGE ( 'NONE', *, *, #8610, .F. ) ;
#403 = CARTESIAN_POINT ( 'NONE',  ( -25.51470164434615029, 30.00000000000000000, 5.000000000000010658 ) ) ;
#404 = VECTOR ( 'NONE', #5914, 1000.000000000000000 ) ;
#405 = CIRCLE ( 'NONE', #6383, 25.00000000000000000 ) ;
#406 = ORIENTED_EDGE ( 'NONE', *, *, #5172, .F. ) ;
#407 = CARTESIAN_POINT ( 'NONE',  ( 32.89361530837994962, 59.92713194881500982, 8.062309845534587183 ) ) ;
#408 = ORIENTED_EDGE ( 'NONE', *, *, #8224, .T. ) ;
#409 = CARTESIAN_POINT ( 'NONE',  ( -5.034526734170375661, -14.99999999999968026, 36.79137236871326877 ) ) ;
#410 = ORIENTED_EDGE ( 'NONE', *, *, #3584, .F. ) ;
#411 = EDGE_CURVE ( 'NONE', #4511, #7590, #7183, .T. ) ;
#412 = EDGE_CURVE ( 'NONE', #8367, #8213, #1224, .T. ) ;
#413 = CARTESIAN_POINT ( 'NONE',  ( -9.860132971832692661, 39.99999999999999289, -28.33333333333334281 ) ) ;
#414 = AXIS2_PLACEMENT_3D ( 'NONE', #5920, #5869, #2063 ) ;
#415 = AXIS2_PLACEMENT_3D ( 'NONE', #8024, #2135, #528 ) ;
#416 = CARTESIAN_POINT ( 'NONE',  ( 2.021687836487040535, 2.655529440325959183E-32, -2.168404344971008868E-16 ) ) ;
#417 = AXIS2_PLACEMENT_3D ( 'NONE', #6684, #4224, #278 ) ;
#418 = AXIS2_PLACEMENT_3D ( 'NONE', #5812, #3538, #4432 ) ;
#419 = AXIS2_PLACEMENT_3D ( 'NONE', #5362, #8372, #1607 ) ;
#420 = CARTESIAN_POINT ( 'NONE',  ( 0.2877257019632035728, 13.29444216721321403, 38.99993006065623291 ) ) ;
#421 = DIRECTION ( 'NONE',  ( -1.000000000000000000, 7.948108874553215112E-17, -6.954033927195823517E-15 ) ) ;
#422 = DIRECTION ( 'NONE',  ( 0.000000000000000000, 0.000000000000000000, -1.000000000000000000 ) ) ;
#423 = CARTESIAN_POINT ( 'NONE',  ( -3.999999999999998224, 0.000000000000000000, 29.00000000000000355 ) ) ;
#424 = ORIENTED_EDGE ( 'NONE', *, *, #837, .F. ) ;
#425 = CARTESIAN_POINT ( 'NONE',  ( 1.300000000000000044, 0.000000000000000000, 0.000000000000000000 ) ) ;
#426 = AXIS2_PLACEMENT_3D ( 'NONE', #882, #3183, #242 ) ;
#427 = VERTEX_POINT ( 'NONE', #5125 ) ;
#428 = DIRECTION ( 'NONE',  ( 0.000000000000000000, 0.000000000000000000, 1.000000000000000000 ) ) ;
#429 = CIRCLE ( 'NONE', #5919, 34.49999999999998579 ) ;
#430 = ORIENTED_EDGE ( 'NONE', *, *, #1372, .T. ) ;
#431 = ADVANCED_FACE ( 'NONE', ( #676 ), #2230, .F. ) ;
#432 = CARTESIAN_POINT ( 'NONE',  ( -8.138638753224961775, -2.524951670102972834, 42.27347557256990029 ) ) ;
#433 = CYLINDRICAL_SURFACE ( 'NONE', #5292, 4.500000000000003553 ) ;
#434 = LINE ( 'NONE', #4865, #3505 ) ;
#435 = CIRCLE ( 'NONE', #6247, 1.500000000000003109 ) ;
#436 = PRODUCT_DEFINITION ( 'UNKNOWN', '', #6631, #7162 ) ;
#437 = ORIENTED_EDGE ( 'NONE', *, *, #7689, .F. ) ;
#438 = FACE_OUTER_BOUND ( 'NONE', #6312, .T. ) ;
#439 = FACE_OUTER_BOUND ( 'NONE', #470, .T. ) ;
#440 = EDGE_LOOP ( 'NONE', ( #9334, #387, #3842, #4081 ) ) ;
#441 = DIRECTION ( 'NONE',  ( 0.000000000000000000, 0.000000000000000000, 1.000000000000000000 ) ) ;
#442 = DIRECTION ( 'NONE',  ( -0.000000000000000000, 1.000000000000000000, -0.000000000000000000 ) ) ;
#443 = CARTESIAN_POINT ( 'NONE',  ( 26.32489316217636954, -15.00000000000000000, -6.000000000000006217 ) ) ;
#444 = CARTESIAN_POINT ( 'NONE',  ( 0.000000000000000000, 61.99999999999999289, 0.000000000000000000 ) ) ;
#445 = FACE_OUTER_BOUND ( 'NONE', #6404, .T. ) ;
#446 = ORIENTED_EDGE ( 'NONE', *, *, #6627, .T. ) ;
#447 = DIRECTION ( 'NONE',  ( -0.000000000000000000, 1.000000000000000000, -0.000000000000000000 ) ) ;
#448 = DIRECTION ( 'NONE',  ( 0.000000000000000000, 0.7071067811865474617, 0.7071067811865474617 ) ) ;
#449 = EDGE_LOOP ( 'NONE', ( #4120, #8855, #5186, #6580 ) ) ;
#450 = DIRECTION ( 'NONE',  ( 0.000000000000000000, 0.000000000000000000, 1.000000000000000000 ) ) ;
#451 = DIRECTION ( 'NONE',  ( -1.735493991486225972E-29, 6.508102468073347395E-30, 1.000000000000000000 ) ) ;
#452 = DIRECTION ( 'NONE',  ( 0.7071067811865573427, -0.7071067811865376918, -0.000000000000000000 ) ) ;
#453 = DIRECTION ( 'NONE',  ( 0.000000000000000000, 0.000000000000000000, -1.000000000000000000 ) ) ;
#454 = EDGE_CURVE ( 'NONE', #4849, #1467, #8923, .T. ) ;
#455 = DIRECTION ( 'NONE',  ( 0.000000000000000000, 1.000000000000000000, 0.000000000000000000 ) ) ;
#456 = ORIENTED_EDGE ( 'NONE', *, *, #4265, .F. ) ;
#457 = DIRECTION ( 'NONE',  ( 0.000000000000000000, 0.000000000000000000, -1.000000000000000000 ) ) ;
#458 = CARTESIAN_POINT ( 'NONE',  ( -5.494756711108470526, -15.00000000000000000, 28.77837652729955309 ) ) ;
#459 = ORIENTED_EDGE ( 'NONE', *, *, #1954, .T. ) ;
#460 = DIRECTION ( 'NONE',  ( 0.6195972517514876099, -0.000000000000000000, 0.7849198975831889191 ) ) ;
#461 = DIRECTION ( 'NONE',  ( -1.000000000000000000, -0.000000000000000000, -0.000000000000000000 ) ) ;
#462 = CARTESIAN_POINT ( 'NONE',  ( 1.388289885975153126, 13.20576465663912735, 38.98465863473316517 ) ) ;
#463 = EDGE_CURVE ( 'NONE', #6976, #7794, #626, .T. ) ;
#464 = EDGE_CURVE ( 'NONE', #7542, #9099, #8278, .T. ) ;
#465 =( NAMED_UNIT ( * ) PLANE_ANGLE_UNIT ( ) SI_UNIT ( $, .RADIAN. ) );
#466 = ORIENTED_EDGE ( 'NONE', *, *, #4986, .F. ) ;
#467 = LINE ( 'NONE', #608, #6068 ) ;
#468 = EDGE_CURVE ( 'NONE', #5208, #1296, #1199, .T. ) ;
#469 = B_SPLINE_CURVE_WITH_KNOTS ( 'NONE', 3,
 ( #5765, #5813, #7291, #4243, #5075, #9572, #1227, #2791, #8825, #7945, #8085, #8782, #1175, #6496, #7140, #6403, #7195, #5857, #2003, #1322, #493, #8877, #4342, #6592, #9613, #9430, #5024, #2641 ),
 .UNSPECIFIED., .F., .F.,
 ( 4, 2, 2, 2, 2, 2, 2, 2, 2, 2, 2, 2, 2, 4 ),
 ( 0.01587631186740470074, 0.01686737684520415656, 0.01785844182300361585, 0.01984057177860253096, 0.02083163675640198678, 0.02182270173420144607, 0.02281376671200090189, 0.02380483168980036118, 0.02578696164539927629, 0.02677802662319873211, 0.02776909160099819140, 0.02975122155659710305, 0.03074228653439655887, 0.03173335151219601469 ),
 .UNSPECIFIED. ) ;
#470 = EDGE_LOOP ( 'NONE', ( #5916, #4580, #3218, #2134, #8926 ) ) ;
#471 = DIRECTION ( 'NONE',  ( 0.9444444444444359821, 0.000000000000000000, -0.3286710990611142469 ) ) ;
#472 = EDGE_LOOP ( 'NONE', ( #7982, #7930, #8063, #3856 ) ) ;
#473 = ORIENTED_EDGE ( 'NONE', *, *, #8224, .F. ) ;
#474 = CARTESIAN_POINT ( 'NONE',  ( -0.4121298502407076403, 18.29573530757822653, 39.00026676411541615 ) ) ;
#475 = DIRECTION ( 'NONE',  ( -0.000000000000000000, -1.000000000000000000, -0.000000000000000000 ) ) ;
#476 = DIRECTION ( 'NONE',  ( -1.224646799147354440E-16, 0.000000000000000000, -1.000000000000000000 ) ) ;
#477 = AXIS2_PLACEMENT_3D ( 'NONE', #8724, #3437, #4921 ) ;
#478 = VERTEX_POINT ( 'NONE', #8225 ) ;
#479 = DIRECTION ( 'NONE',  ( 0.000000000000000000, 0.000000000000000000, 1.000000000000000000 ) ) ;
#480 = EDGE_CURVE ( 'NONE', #2405, #7052, #1136, .T. ) ;
#481 = ORIENTED_EDGE ( 'NONE', *, *, #7790, .F. ) ;
#482 = CARTESIAN_POINT ( 'NONE',  ( -8.216777476527274970, 48.50000000000033396, -23.61111111111111427 ) ) ;
#483 = FACE_OUTER_BOUND ( 'NONE', #5558, .T. ) ;
#484 = CARTESIAN_POINT ( 'NONE',  ( 10.76768976630624763, 12.19644567871079488, 37.49298203710821298 ) ) ;
#485 = CARTESIAN_POINT ( 'NONE',  ( 2.400000000000000799, 0.000000000000000000, 0.000000000000000000 ) ) ;
#486 = CARTESIAN_POINT ( 'NONE',  ( -5.999999999999998224, -15.00000000000000000, 31.00000000000000711 ) ) ;
#487 = CIRCLE ( 'NONE', #5977, 29.00000000000001776 ) ;
#488 = CARTESIAN_POINT ( 'NONE',  ( 1.555535097482682654E-26, 78.08723716182652197, -25.00000000000000000 ) ) ;
#489 = ORIENTED_EDGE ( 'NONE', *, *, #3270, .T. ) ;
#490 = SHAPE_REPRESENTATION ( 'socket button head screw_iso_ISO 7380 - M4 x 10 - 10N', ( #6314 ), #6474 ) ;
#491 = DIRECTION ( 'NONE',  ( 0.000000000000000000, 0.000000000000000000, 1.000000000000000000 ) ) ;
#492 = AXIS2_PLACEMENT_3D ( 'NONE', #3896, #148, #8677 ) ;
#493 = CARTESIAN_POINT ( 'NONE',  ( 4.177119896625375972, 12.38650817078062083, 43.55397297161687220 ) ) ;
#494 = EDGE_LOOP ( 'NONE', ( #6497, #4079, #9500, #4446, #1743, #1658, #5716 ) ) ;
#495 = PLANE ( 'NONE',  #7443 ) ;
#496 = DIRECTION ( 'NONE',  ( -0.9860132971832694659, -1.788557213313974350E-28, 0.1666666666666658247 ) ) ;
#497 = CARTESIAN_POINT ( 'NONE',  ( 7.710389085651311980, -7.163490336350744059, 38.44899322361341376 ) ) ;
#498 = COLOUR_RGB ( '',0.7921568627450980005, 0.8196078431372548767, 0.9333333333333333481 ) ;
#499 = DIRECTION ( 'NONE',  ( 0.000000000000000000, 0.000000000000000000, 1.000000000000000000 ) ) ;
#500 = PRODUCT_DEFINITION_FORMATION_WITH_SPECIFIED_SOURCE ( 'ANY', '', #4115, .NOT_KNOWN. ) ;
#501 = ORIENTED_EDGE ( 'NONE', *, *, #2623, .T. ) ;
#502 = FACE_BOUND ( 'NONE', #5683, .T. ) ;
#503 = CARTESIAN_POINT ( 'NONE',  ( -2.609644126788640328, -9.208034112191455733, 39.41000430683886435 ) ) ;
#504 = VERTEX_POINT ( 'NONE', #5174 ) ;
#505 = CARTESIAN_POINT ( 'NONE',  ( 6.000000000000001776, 27.42469319230600533, -31.00000000000000711 ) ) ;
#506 = CARTESIAN_POINT ( 'NONE',  ( 30.18708036726505028, 60.99999999999999289, 16.70299909897265778 ) ) ;
#507 = CARTESIAN_POINT ( 'NONE',  ( 8.142856695446859305, 15.19239146806992125, 38.14742590042245496 ) ) ;
#508 = DIRECTION ( 'NONE',  ( 6.954033927195823517E-15, -5.551115123125807354E-17, -1.000000000000000000 ) ) ;
#509 = EDGE_CURVE ( 'NONE', #4792, #7168, #1410, .T. ) ;
#510 = ADVANCED_FACE ( 'NONE', ( #144 ), #7240, .F. ) ;
#511 = CIRCLE ( 'NONE', #8869, 5.000000000000001776 ) ;
#512 = VECTOR ( 'NONE', #9362, 1000.000000000000000 ) ;
#513 = ORIENTED_EDGE ( 'NONE', *, *, #7286, .F. ) ;
#514 = CARTESIAN_POINT ( 'NONE',  ( 0.000000000000000000, 30.00000000000000000, 0.000000000000000000 ) ) ;
#515 = CARTESIAN_POINT ( 'NONE',  ( 3.885274725274726393, -8.673617379884035472E-16, 0.000000000000000000 ) ) ;
#516 = CARTESIAN_POINT ( 'NONE',  ( -4.000000000000005329, 28.99999999999997158, -29.00000000000000355 ) ) ;
#517 = VERTEX_POINT ( 'NONE', #5126 ) ;
#518 = EDGE_LOOP ( 'NONE', ( #1786, #1861, #2119, #8803 ) ) ;
#519 = B_SPLINE_CURVE_WITH_KNOTS ( 'NONE', 3,
 ( #6161, #3804, #5389, #1530 ),
 .UNSPECIFIED., .F., .F.,
 ( 4, 4 ),
 ( 9.813077866773594792E-18, 0.003679109433542027217 ),
 .UNSPECIFIED. ) ;
#520 = CARTESIAN_POINT ( 'NONE',  ( -5.000088184532109459, 11.96127634219708291, 43.35829465038302999 ) ) ;
#521 = EDGE_CURVE ( 'NONE', #3666, #5938, #5175, .T. ) ;
#522 = DIRECTION ( 'NONE',  ( -0.7849198975831889191, -0.000000000000000000, 0.6195972517514874989 ) ) ;
#523 = AXIS2_PLACEMENT_3D ( 'NONE', #9479, #3779, #453 ) ;
#524 = ADVANCED_FACE ( 'NONE', ( #4341 ), #7345, .F. ) ;
#525 = DIRECTION ( 'NONE',  ( 0.000000000000000000, 1.000000000000000000, 0.000000000000000000 ) ) ;
#526 = EDGE_CURVE ( 'NONE', #1263, #8611, #8767, .T. ) ;
#527 = ORIENTED_EDGE ( 'NONE', *, *, #2371, .T. ) ;
#528 = DIRECTION ( 'NONE',  ( 0.000000000000000000, 0.000000000000000000, -1.000000000000000000 ) ) ;
#529 = CARTESIAN_POINT ( 'NONE',  ( 28.33333333333337833, 59.99999999999999289, -9.860132971832594961 ) ) ;
#530 = ORIENTED_EDGE ( 'NONE', *, *, #3207, .T. ) ;
#531 = CARTESIAN_POINT ( 'NONE',  ( 4.000000000000001776, 0.000000000000000000, 0.000000000000000000 ) ) ;
#532 = VECTOR ( 'NONE', #9646, 1000.000000000000341 ) ;
#533 = VECTOR ( 'NONE', #5958, 1000.000000000000000 ) ;
#534 = LINE ( 'NONE', #2734, #9462 ) ;
#535 = EDGE_CURVE ( 'NONE', #4621, #5147, #2943, .T. ) ;
#536 = CARTESIAN_POINT ( 'NONE',  ( 8.924601364836032502, 14.41850173042159433, 37.96585739592215702 ) ) ;
#537 = CARTESIAN_POINT ( 'NONE',  ( 33.06426808735054124, 60.99999999999999289, 10.06230984553459251 ) ) ;
#538 = EDGE_CURVE ( 'NONE', #6765, #4792, #5901, .T. ) ;
#539 = CARTESIAN_POINT ( 'NONE',  ( -28.37252191822215863, 30.00000000000000000, 6.000000000000009770 ) ) ;
#540 = ADVANCED_FACE ( 'NONE', ( #4241, #5074 ), #1370, .F. ) ;
#541 = ADVANCED_FACE ( 'NONE', ( #6547 ), #5764, .T. ) ;
#542 = AXIS2_PLACEMENT_3D ( 'NONE', #8748, #5544, #7870 ) ;
#543 = EDGE_LOOP ( 'NONE', ( #1051, #1882 ) ) ;
#544 = CARTESIAN_POINT ( 'NONE',  ( 5.423418723394456162E-28, -2.066522830327504070E-28, -26.00000000000000355 ) ) ;
#545 = DIRECTION ( 'NONE',  ( 1.735493991486223450E-29, 0.000000000000000000, -1.000000000000000000 ) ) ;
#546 = EDGE_LOOP ( 'NONE', ( #4268, #589, #822, #6096, #5200 ) ) ;
#547 = FACE_OUTER_BOUND ( 'NONE', #7373, .T. ) ;
#548 = LINE ( 'NONE', #5078, #2613 ) ;
#549 = DIRECTION ( 'NONE',  ( 0.000000000000000000, -1.000000000000000000, 0.000000000000000000 ) ) ;
#550 = CARTESIAN_POINT ( 'NONE',  ( 11.07761026121386294, -5.000000000000018652, 37.39366993089406321 ) ) ;
#551 = SHAPE_REPRESENTATION ( 'Metal Body for Mounting Threaded Chasers', ( #6314 ), #2843 ) ;
#552 = CARTESIAN_POINT ( 'NONE',  ( 0.000000000000000000, 60.99999999999999289, 0.000000000000000000 ) ) ;
#553 = EDGE_CURVE ( 'NONE', #1486, #2396, #9731, .T. ) ;
#554 = ORIENTED_EDGE ( 'NONE', *, *, #4928, .F. ) ;
#555 = DIRECTION ( 'NONE',  ( -0.000000000000000000, -1.000000000000000000, -0.000000000000000000 ) ) ;
#556 = CARTESIAN_POINT ( 'NONE',  ( 0.1989820186609699559, -14.99999999999991829, 36.76396650344398864 ) ) ;
#557 = ORIENTED_EDGE ( 'NONE', *, *, #2320, .F. ) ;
#558 = DIRECTION ( 'NONE',  ( -0.000000000000000000, -1.000000000000000000, -0.000000000000000000 ) ) ;
#559 = CARTESIAN_POINT ( 'NONE',  ( 2.400000000000000799, 0.000000000000000000, 0.000000000000000000 ) ) ;
#560 = CARTESIAN_POINT ( 'NONE',  ( 4.161522685292555757, 12.39367310823792145, 43.55734157098922310 ) ) ;
#561 = CARTESIAN_POINT ( 'NONE',  ( -33.06426808735054834, 63.19999999999998153, -5.562309845534567643 ) ) ;
#562 = ORIENTED_EDGE ( 'NONE', *, *, #6925, .F. ) ;
#563 = CARTESIAN_POINT ( 'NONE',  ( -34.19425402209839859, 59.81545713833158828, -3.326151553796970806 ) ) ;
#564 = ORIENTED_EDGE ( 'NONE', *, *, #4438, .T. ) ;
#565 = CARTESIAN_POINT ( 'NONE',  ( 33.72911585420148128, 59.92558239856793278, 3.146586008005429314 ) ) ;
#566 = ORIENTED_EDGE ( 'NONE', *, *, #352, .T. ) ;
#567 = CARTESIAN_POINT ( 'NONE',  ( 0.000000000000000000, 52.29648987751954792, -38.00000000000000711 ) ) ;
#568 = ORIENTED_EDGE ( 'NONE', *, *, #7347, .T. ) ;
#569 = AXIS2_PLACEMENT_3D ( 'NONE', #6747, #8347, #8246 ) ;
#570 = CARTESIAN_POINT ( 'NONE',  ( -5.877770207244633838, 16.75843190384220804, 38.55650392976755114 ) ) ;
#571 = AXIS2_PLACEMENT_3D ( 'NONE', #1883, #7968, #2471 ) ;
#572 = FACE_OUTER_BOUND ( 'NONE', #3011, .T. ) ;
#573 = AXIS2_PLACEMENT_3D ( 'NONE', #9355, #2572, #5602 ) ;
#574 = EDGE_CURVE ( 'NONE', #9611, #2873, #3443, .T. ) ;
#575 = DIRECTION ( 'NONE',  ( 0.000000000000000000, -0.7071067811865500152, -0.7071067811865451302 ) ) ;
#576 = CONICAL_SURFACE ( 'NONE', #6079, 10.00000000000001421, 0.07734202994352787353 ) ;
#577 = VERTEX_POINT ( 'NONE', #6443 ) ;
#578 = CARTESIAN_POINT ( 'NONE',  ( 7.913260955498274673E-27, 41.50000000000020606, -26.00000000000017408 ) ) ;
#579 = ORIENTED_EDGE ( 'NONE', *, *, #6665, .T. ) ;
#580 = DIRECTION ( 'NONE',  ( -1.820952055660014662E-28, -1.000000000000000000, -7.038118388768679669E-30 ) ) ;
#581 = CARTESIAN_POINT ( 'NONE',  ( 0.000000000000000000, 30.00000000000000000, 0.000000000000000000 ) ) ;
#582 = CARTESIAN_POINT ( 'NONE',  ( 0.000000000000000000, 60.99999999999999289, 0.000000000000000000 ) ) ;
#583 = DIRECTION ( 'NONE',  ( 0.000000000000000000, 0.000000000000000000, -1.000000000000000000 ) ) ;
#584 = CIRCLE ( 'NONE', #9564, 2.500000000000002220 ) ;
#585 = CARTESIAN_POINT ( 'NONE',  ( 4.331874290630496560, 29.33187429063046991, 24.96033808169876878 ) ) ;
#586 = EDGE_CURVE ( 'NONE', #9099, #2192, #627, .T. ) ;
#587 = VECTOR ( 'NONE', #9325, 1000.000000000000000 ) ;
#588 = ADVANCED_FACE ( 'NONE', ( #8138 ), #2885, .T. ) ;
#589 = ORIENTED_EDGE ( 'NONE', *, *, #6961, .T. ) ;
#590 = DIRECTION ( 'NONE',  ( -1.000000000000000000, 0.000000000000000000, 2.168404344971006649E-16 ) ) ;
#591 = DIRECTION ( 'NONE',  ( 0.000000000000000000, 1.000000000000000000, 0.000000000000000000 ) ) ;
#592 = EDGE_CURVE ( 'NONE', #7004, #2792, #2691, .T. ) ;
#593 = ORIENTED_EDGE ( 'NONE', *, *, #4388, .T. ) ;
#594 = CARTESIAN_POINT ( 'NONE',  ( -4.904043666719616112, 61.99999999999999289, -31.11591804390330651 ) ) ;
#595 = DIRECTION ( 'NONE',  ( 0.000000000000000000, 1.000000000000000000, 0.000000000000000000 ) ) ;
#596 = DIRECTION ( 'NONE',  ( -0.000000000000000000, -1.000000000000000000, -0.000000000000000000 ) ) ;
#597 = DIRECTION ( 'NONE',  ( -1.000000000000000000, -0.000000000000000000, -0.000000000000000000 ) ) ;
#598 = ORIENTED_EDGE ( 'NONE', *, *, #5533, .T. ) ;
#599 = CARTESIAN_POINT ( 'NONE',  ( -8.216777476527274970, 47.50000000000033396, -23.61111111111111427 ) ) ;
#600 = FACE_OUTER_BOUND ( 'NONE', #8417, .T. ) ;
#601 = EDGE_LOOP ( 'NONE', ( #1791, #2540, #7807, #3145, #4063 ) ) ;
#602 = CARTESIAN_POINT ( 'NONE',  ( -9.860132971832692661, 59.99999999999999289, -28.33333333333334281 ) ) ;
#603 = DIRECTION ( 'NONE',  ( 0.000000000000000000, 0.000000000000000000, 1.000000000000000000 ) ) ;
#604 = EDGE_LOOP ( 'NONE', ( #4455, #8847, #6470, #2076 ) ) ;
#605 = CARTESIAN_POINT ( 'NONE',  ( 11.29943480391912480, 11.21459584331072712, 37.32807029000129972 ) ) ;
#606 = DIRECTION ( 'NONE',  ( 1.180727526274980869E-14, 2.263060015900834493E-17, 1.000000000000000000 ) ) ;
#607 = EDGE_LOOP ( 'NONE', ( #895, #6657 ) ) ;
#608 = CARTESIAN_POINT ( 'NONE',  ( 1.040310318760209318E-26, 47.00000000000034106, -37.00000000000000711 ) ) ;
#609 = ORIENTED_EDGE ( 'NONE', *, *, #1964, .F. ) ;
#610 = LINE ( 'NONE', #1297, #1967 ) ;
#611 = ORIENTED_EDGE ( 'NONE', *, *, #2805, .F. ) ;
#612 = PLANE ( 'NONE',  #732 ) ;
#613 = ORIENTED_EDGE ( 'NONE', *, *, #7697, .F. ) ;
#614 = CARTESIAN_POINT ( 'NONE',  ( -10.79121869663144651, 12.07057269213421691, 37.47816149638868666 ) ) ;
#615 = CARTESIAN_POINT ( 'NONE',  ( 9.860761315262647568E-27, 50.00000000000032685, -24.09806918451531033 ) ) ;
#616 = CARTESIAN_POINT ( 'NONE',  ( -8.216777476527274970, 78.08723716182652197, -23.61111111111111427 ) ) ;
#617 = EDGE_LOOP ( 'NONE', ( #366, #613, #1994, #8826 ) ) ;
#618 = CARTESIAN_POINT ( 'NONE',  ( -16.70299909897276081, 61.99999999999999289, 30.18708036726496857 ) ) ;
#619 = ORIENTED_EDGE ( 'NONE', *, *, #8790, .F. ) ;
#620 = FACE_OUTER_BOUND ( 'NONE', #3521, .T. ) ;
#621 = DIRECTION ( 'NONE',  ( 0.000000000000000000, -1.000000000000000000, 0.000000000000000000 ) ) ;
#622 = DIRECTION ( 'NONE',  ( 0.000000000000000000, 0.000000000000000000, 1.000000000000000000 ) ) ;
#623 = DIRECTION ( 'NONE',  ( 0.3271946967961529840, 0.000000000000000000, -0.9449569463147373671 ) ) ;
#624 = DIRECTION ( 'NONE',  ( -0.000000000000000000, -1.000000000000000000, -0.000000000000000000 ) ) ;
#625 = ORIENTED_EDGE ( 'NONE', *, *, #1724, .T. ) ;
#626 = LINE ( 'NONE', #5323, #2764 ) ;
#627 = LINE ( 'NONE', #6495, #5483 ) ;
#628 = DIRECTION ( 'NONE',  ( 1.735493991486225692E-29, 0.000000000000000000, -1.000000000000000000 ) ) ;
#629 = PLANE ( 'NONE',  #8412 ) ;
#630 = DIRECTION ( 'NONE',  ( 0.000000000000000000, 1.000000000000000000, 0.000000000000000000 ) ) ;
#631 = VECTOR ( 'NONE', #3107, 1000.000000000000000 ) ;
#632 = AXIS2_PLACEMENT_3D ( 'NONE', #9012, #5209, #2137 ) ;
#633 = CARTESIAN_POINT ( 'NONE',  ( 0.000000000000000000, -1.443375672974064328, -9.326206579303807412E-18 ) ) ;
#634 = ADVANCED_FACE ( 'NONE', ( #4391 ), #5023, .F. ) ;
#635 = EDGE_CURVE ( 'NONE', #5898, #2818, #5499, .T. ) ;
#636 = ADVANCED_FACE ( 'NONE', ( #9571 ), #1321, .T. ) ;
#637 = AXIS2_PLACEMENT_3D ( 'NONE', #6190, #2432, #823 ) ;
#638 = LINE ( 'NONE', #8740, #6512 ) ;
#639 = CARTESIAN_POINT ( 'NONE',  ( 0.000000000000000000, 52.29648987751954792, -40.00000000000000711 ) ) ;
#640 = ORIENTED_EDGE ( 'NONE', *, *, #8427, .F. ) ;
#641 = CARTESIAN_POINT ( 'NONE',  ( 31.00000000000000711, -10.00000000000000533, -6.000000000000006217 ) ) ;
#642 = CARTESIAN_POINT ( 'NONE',  ( 6.848559158582876449, -14.99999999999999822, 28.25275382443572525 ) ) ;
#643 = ORIENTED_EDGE ( 'NONE', *, *, #1715, .F. ) ;
#644 = AXIS2_PLACEMENT_3D ( 'NONE', #4878, #3192, #6296 ) ;
#645 = AXIS2_PLACEMENT_3D ( 'NONE', #194, #4729, #6198 ) ;
#646 = EDGE_CURVE ( 'NONE', #1381, #4052, #9276, .T. ) ;
#647 = DIRECTION ( 'NONE',  ( 1.735493991486224571E-29, 0.000000000000000000, -1.000000000000000000 ) ) ;
#648 = CARTESIAN_POINT ( 'NONE',  ( 9.762153702110021092E-27, 45.50000000000019185, -37.00000000000000711 ) ) ;
#649 = EDGE_CURVE ( 'NONE', #2857, #6423, #145, .T. ) ;
#650 = CARTESIAN_POINT ( 'NONE',  ( 9.569793796949216613, 0.3522634836077675469, 37.96578825203867780 ) ) ;
#651 = APPLICATION_PROTOCOL_DEFINITION ( 'draft international standard', 'automotive_design', 1998, #1076 ) ;
#652 = AXIS2_PLACEMENT_3D ( 'NONE', #8214, #4323, #7326 ) ;
#653 = AXIS2_PLACEMENT_3D ( 'NONE', #663, #4395, #7445 ) ;
#654 = ORIENTED_EDGE ( 'NONE', *, *, #4759, .F. ) ;
#655 = DIRECTION ( 'NONE',  ( 0.000000000000000000, 0.000000000000000000, 1.000000000000000000 ) ) ;
#656 = EDGE_LOOP ( 'NONE', ( #2206, #5652, #8813, #128, #3194 ) ) ;
#657 = CARTESIAN_POINT ( 'NONE',  ( 35.48172963891341425, 59.13032414405947179, 4.904055200121585578 ) ) ;
#658 = ORIENTED_EDGE ( 'NONE', *, *, #8055, .F. ) ;
#659 = DIRECTION ( 'NONE',  ( -1.820952055660014662E-28, -1.000000000000000000, -7.038118388768679669E-30 ) ) ;
#660 = ORIENTED_EDGE ( 'NONE', *, *, #3351, .F. ) ;
#661 = CARTESIAN_POINT ( 'NONE',  ( -6.789484220152367300, 10.67953771436871691, 38.52138918282914659 ) ) ;
#662 = DIRECTION ( 'NONE',  ( 0.000000000000000000, 1.000000000000000000, 0.000000000000000000 ) ) ;
#663 = CARTESIAN_POINT ( 'NONE',  ( 1.555535097482682654E-26, 78.08723716182652197, -25.00000000000000000 ) ) ;
#664 = LINE ( 'NONE', #4320, #1771 ) ;
#665 = VECTOR ( 'NONE', #3132, 1000.000000000000000 ) ;
#666 = ORIENTED_EDGE ( 'NONE', *, *, #2923, .F. ) ;
#667 = VERTEX_POINT ( 'NONE', #3684 ) ;
#668 = EDGE_CURVE ( 'NONE', #2236, #5750, #3130, .T. ) ;
#669 = DIRECTION ( 'NONE',  ( 1.000000000000000000, 0.000000000000000000, 0.000000000000000000 ) ) ;
#670 = DIRECTION ( 'NONE',  ( 0.000000000000000000, 0.000000000000000000, 1.000000000000000000 ) ) ;
#671 = AXIS2_PLACEMENT_3D ( 'NONE', #7509, #58, #2953 ) ;
#672 = DIRECTION ( 'NONE',  ( 1.735493991486225411E-29, 0.000000000000000000, -1.000000000000000000 ) ) ;
#673 = AXIS2_PLACEMENT_3D ( 'NONE', #8739, #2698, #4205 ) ;
#674 = CARTESIAN_POINT ( 'NONE',  ( 0.000000000000000000, 54.99999999999999289, 0.000000000000000000 ) ) ;
#675 = ORIENTED_EDGE ( 'NONE', *, *, #3911, .F. ) ;
#676 = FACE_OUTER_BOUND ( 'NONE', #8642, .T. ) ;
#677 = LINE ( 'NONE', #6683, #1670 ) ;
#678 = DIRECTION ( 'NONE',  ( -0.000000000000000000, 1.000000000000000000, -0.000000000000000000 ) ) ;
#679 = CARTESIAN_POINT ( 'NONE',  ( -32.59762842694629370, 61.99999999999999289, 5.137569555611143812 ) ) ;
#680 = DIRECTION ( 'NONE',  ( 0.000000000000000000, 0.000000000000000000, 1.000000000000000000 ) ) ;
#681 = CARTESIAN_POINT ( 'NONE',  ( -31.00000000000001066, 28.00044749928606791, 0.9877776005181286845 ) ) ;
#682 = CIRCLE ( 'NONE', #6188, 2.000000000000000000 ) ;
#683 = VECTOR ( 'NONE', #8096, 1000.000000000000000 ) ;
#684 = EDGE_CURVE ( 'NONE', #7011, #7381, #677, .T. ) ;
#685 = B_SPLINE_CURVE_WITH_KNOTS ( 'NONE', 3,
 ( #9148, #1636, #3056, #5346 ),
 .UNSPECIFIED., .F., .F.,
 ( 4, 4 ),
 ( 0.000000000000000000, 0.001643226871903046308 ),
 .UNSPECIFIED. ) ;
#686 = PLANE ( 'NONE',  #5828 ) ;
#687 = CARTESIAN_POINT ( 'NONE',  ( 20.99999999999999645, 30.00000000000000000, -4.000000000000006217 ) ) ;
#688 = EDGE_LOOP ( 'NONE', ( #2555, #5795, #446, #121 ) ) ;
#689 = LINE ( 'NONE', #2993, #4805 ) ;
#690 = EDGE_CURVE ( 'NONE', #5689, #4621, #1513, .T. ) ;
#691 = ORIENTED_EDGE ( 'NONE', *, *, #2255, .T. ) ;
#692 = DIRECTION ( 'NONE',  ( 0.000000000000000000, 1.000000000000000000, 0.000000000000000000 ) ) ;
#693 = CARTESIAN_POINT ( 'NONE',  ( 3.829830809861694441, -15.00000000000031619, 36.77956184265733697 ) ) ;
#694 = EDGE_CURVE ( 'NONE', #9443, #2001, #5462, .T. ) ;
#695 = ORIENTED_EDGE ( 'NONE', *, *, #6119, .T. ) ;
#696 = CARTESIAN_POINT ( 'NONE',  ( 1.300000000000000044, 0.7216878364870328300, 1.250000000000000000 ) ) ;
#697 = LINE ( 'NONE', #6703, #2761 ) ;
#698 = ORIENTED_EDGE ( 'NONE', *, *, #2685, .T. ) ;
#699 = CIRCLE ( 'NONE', #1016, 4.500000000000005329 ) ;
#700 = ORIENTED_EDGE ( 'NONE', *, *, #4695, .T. ) ;
#701 = CARTESIAN_POINT ( 'NONE',  ( 1.002605232869780806E-26, 55.00000000000030553, 3.131562089573645497E-28 ) ) ;
#702 = ADVANCED_FACE ( 'NONE', ( #881 ), #5993, .F. ) ;
#703 = ORIENTED_EDGE ( 'NONE', *, *, #1808, .F. ) ;
#704 = CARTESIAN_POINT ( 'NONE',  ( 35.54672840350796292, 58.97502204235875922, 5.902312647278757929 ) ) ;
#705 = ADVANCED_FACE ( 'NONE', ( #7547 ), #776, .F. ) ;
#706 = ORIENTED_EDGE ( 'NONE', *, *, #9278, .T. ) ;
#707 = DIRECTION ( 'NONE',  ( 0.000000000000000000, 0.000000000000000000, -1.000000000000000000 ) ) ;
#708 = AXIS2_PLACEMENT_3D ( 'NONE', #7091, #1077, #2399 ) ;
#709 = APPLICATION_CONTEXT ( 'automotive_design' ) ;
#710 = EDGE_CURVE ( 'NONE', #1005, #1238, #6143, .T. ) ;
#711 = EDGE_LOOP ( 'NONE', ( #4221, #2161, #4934, #4957, #6130 ) ) ;
#712 = DIRECTION ( 'NONE',  ( -0.000000000000000000, -1.000000000000000000, -0.000000000000000000 ) ) ;
#713 = CARTESIAN_POINT ( 'NONE',  ( -8.545448575588398654, 44.00000000000019895, -24.55555555555570990 ) ) ;
#714 = DIRECTION ( 'NONE',  ( 1.000000000000000000, 0.000000000000000000, 0.000000000000000000 ) ) ;
#715 = VECTOR ( 'NONE', #596, 1000.000000000000000 ) ;
#716 = ORIENTED_EDGE ( 'NONE', *, *, #8054, .F. ) ;
#717 = DIRECTION ( 'NONE',  ( 0.000000000000000000, 0.000000000000000000, -1.000000000000000000 ) ) ;
#718 = ORIENTED_EDGE ( 'NONE', *, *, #3473, .F. ) ;
#719 = AXIS2_PLACEMENT_3D ( 'NONE', #3811, #4556, #6908 ) ;
#720 = DIRECTION ( 'NONE',  ( 0.000000000000000000, 0.000000000000000000, -1.000000000000000000 ) ) ;
#721 = CIRCLE ( 'NONE', #90, 26.00000000000004974 ) ;
#722 = DIRECTION ( 'NONE',  ( 0.000000000000000000, 0.000000000000000000, -1.000000000000000000 ) ) ;
#723 =( NAMED_UNIT ( * ) PLANE_ANGLE_UNIT ( ) SI_UNIT ( $, .RADIAN. ) );
#724 = CARTESIAN_POINT ( 'NONE',  ( 8.726773764007443097E-27, 41.50000000000020606, -37.00000000000000711 ) ) ;
#725 = VECTOR ( 'NONE', #4013, 1000.000000000000000 ) ;
#726 = AXIS2_PLACEMENT_3D ( 'NONE', #2931, #8863, #5748 ) ;
#727 = AXIS2_PLACEMENT_3D ( 'NONE', #6622, #9643, #2128 ) ;
#728 = CARTESIAN_POINT ( 'NONE',  ( 11.80999999999999872, 0.000000000000000000, 0.000000000000000000 ) ) ;
#729 = ORIENTED_EDGE ( 'NONE', *, *, #5227, .T. ) ;
#730 = DIRECTION ( 'NONE',  ( -1.000000000000000000, 0.000000000000000000, -6.982962677686269077E-15 ) ) ;
#731 = DIRECTION ( 'NONE',  ( 0.000000000000000000, 0.000000000000000000, 1.000000000000000000 ) ) ;
#732 = AXIS2_PLACEMENT_3D ( 'NONE', #5881, #2122, #3614 ) ;
#733 = CARTESIAN_POINT ( 'NONE',  ( -8.216777476527274970, 78.08723716182652197, -23.61111111111111427 ) ) ;
#734 = CARTESIAN_POINT ( 'NONE',  ( -5.000000000000002665, 30.00000000000000000, 5.421010862427519212E-16 ) ) ;
#735 = CARTESIAN_POINT ( 'NONE',  ( -6.704071815732007167, 16.26702755093696240, 38.42308545116613061 ) ) ;
#736 = CIRCLE ( 'NONE', #5785, 40.00000000000000711 ) ;
#737 = LINE ( 'NONE', #9449, #1576 ) ;
#738 = CYLINDRICAL_SURFACE ( 'NONE', #9058, 26.00000000000002132 ) ;
#739 = ORIENTED_EDGE ( 'NONE', *, *, #3429, .F. ) ;
#740 = DIRECTION ( 'NONE',  ( -0.000000000000000000, 1.000000000000000000, -0.000000000000000000 ) ) ;
#741 = CARTESIAN_POINT ( 'NONE',  ( 4.138326062248817827, -15.00000000000031442, 36.78203384243531815 ) ) ;
#742 = VERTEX_POINT ( 'NONE', #2390 ) ;
#743 = DIRECTION ( 'NONE',  ( 0.000000000000000000, 0.000000000000000000, 1.000000000000000000 ) ) ;
#744 = AXIS2_PLACEMENT_3D ( 'NONE', #8928, #8876, #3589 ) ;
#745 = CARTESIAN_POINT ( 'NONE',  ( -5.421010862427522170E-16, 30.00000000000000000, -5.000000000000004441 ) ) ;
#746 = CARTESIAN_POINT ( 'NONE',  ( 0.000000000000000000, 0.000000000000000000, 0.000000000000000000 ) ) ;
#747 = ORIENTED_EDGE ( 'NONE', *, *, #8375, .F. ) ;
#748 = EDGE_CURVE ( 'NONE', #1486, #8507, #3031, .T. ) ;
#749 = EDGE_CURVE ( 'NONE', #4632, #7580, #3329, .T. ) ;
#750 = CARTESIAN_POINT ( 'NONE',  ( 13.27537549950361750, 4.257531348894068479, 36.67105783558309895 ) ) ;
#751 = ORIENTED_EDGE ( 'NONE', *, *, #8313, .F. ) ;
#752 = DIRECTION ( 'NONE',  ( 0.000000000000000000, 1.000000000000000000, 0.000000000000000000 ) ) ;
#753 = DIRECTION ( 'NONE',  ( -0.000000000000000000, 1.000000000000000000, -0.000000000000000000 ) ) ;
#754 = ORIENTED_EDGE ( 'NONE', *, *, #2562, .F. ) ;
#755 = CARTESIAN_POINT ( 'NONE',  ( -26.32489316217636954, 30.00000000000000000, 6.000000000000009770 ) ) ;
#756 = EDGE_LOOP ( 'NONE', ( #6277, #2707, #2259, #1745, #813, #6889 ) ) ;
#757 = CARTESIAN_POINT ( 'NONE',  ( 0.000000000000000000, 54.99999999999999289, 0.000000000000000000 ) ) ;
#758 = DIRECTION ( 'NONE',  ( -0.7071067811865573427, 0.7071067811865376918, 0.000000000000000000 ) ) ;
#759 = CARTESIAN_POINT ( 'NONE',  ( 23.54759692749571087, 59.99999999999999289, -18.58791755254458167 ) ) ;
#760 = EDGE_CURVE ( 'NONE', #4270, #9740, #8481, .T. ) ;
#761 = EDGE_CURVE ( 'NONE', #1456, #8266, #8388, .T. ) ;
#762 = ADVANCED_FACE ( 'NONE', ( #4778 ), #1708, .F. ) ;
#763 = ORIENTED_EDGE ( 'NONE', *, *, #7205, .T. ) ;
#764 = CARTESIAN_POINT ( 'NONE',  ( 32.99503133754566875, 59.99860354191589806, 3.062309845534584074 ) ) ;
#765 = ORIENTED_EDGE ( 'NONE', *, *, #4331, .T. ) ;
#766 = ORIENTED_EDGE ( 'NONE', *, *, #2477, .T. ) ;
#767 = CARTESIAN_POINT ( 'NONE',  ( -28.37252191822216218, 30.00000000000000000, -5.999999999999996447 ) ) ;
#768 = FACE_OUTER_BOUND ( 'NONE', #8392, .T. ) ;
#769 = FACE_OUTER_BOUND ( 'NONE', #3306, .T. ) ;
#770 = ADVANCED_FACE ( 'NONE', ( #7031 ), #5661, .F. ) ;
#771 = ADVANCED_FACE ( 'NONE', ( #8525 ), #8673, .F. ) ;
#772 = ORIENTED_EDGE ( 'NONE', *, *, #7387, .T. ) ;
#773 = CARTESIAN_POINT ( 'NONE',  ( -8.216777476527274970, 78.08723716182652197, -23.61111111111111427 ) ) ;
#774 = EDGE_LOOP ( 'NONE', ( #566, #4057 ) ) ;
#775 = CARTESIAN_POINT ( 'NONE',  ( -7.214865095667844841, 61.84561525624321376, 37.26328141369679514 ) ) ;
#776 = PLANE ( 'NONE',  #7111 ) ;
#777 = CARTESIAN_POINT ( 'NONE',  ( 8.577746286997626155E-27, 47.00000000000034106, 1.660151612061797305E-28 ) ) ;
#778 = CARTESIAN_POINT ( 'NONE',  ( -2.813731784447083495, -15.00000000000000178, 29.91201187495168412 ) ) ;
#779 = CARTESIAN_POINT ( 'NONE',  ( 8.237197373723128990, -15.00000000000000000, 27.80554943579302574 ) ) ;
#780 = LINE ( 'NONE', #7737, #4904 ) ;
#781 = ORIENTED_EDGE ( 'NONE', *, *, #7457, .T. ) ;
#782 = DIRECTION ( 'NONE',  ( 0.000000000000000000, 1.224646799147353207E-16, -1.000000000000000000 ) ) ;
#783 = AXIS2_PLACEMENT_3D ( 'NONE', #4118, #4582, #7112 ) ;
#784 = CIRCLE ( 'NONE', #5829, 33.00000000000000711 ) ;
#785 = DIRECTION ( 'NONE',  ( -1.820952055660014662E-28, -1.000000000000000000, -7.038118388768679669E-30 ) ) ;
#786 = PRODUCT ( 'Covrt plate', 'Covrt plate', '', ( #2257 ) ) ;
#787 = ORIENTED_EDGE ( 'NONE', *, *, #1184, .T. ) ;
#788 = CARTESIAN_POINT ( 'NONE',  ( -5.562309845534584518, 49.99999999999999289, 35.56426808735054834 ) ) ;
#789 = CARTESIAN_POINT ( 'NONE',  ( 3.173702698177182313, -14.99999999999968736, 36.77512248518149107 ) ) ;
#790 = EDGE_CURVE ( 'NONE', #2152, #2914, #4725, .T. ) ;
#791 = ORIENTED_EDGE ( 'NONE', *, *, #3597, .T. ) ;
#792 = CARTESIAN_POINT ( 'NONE',  ( 5.137569555611264605, 60.99999999999999289, 32.59762842694627949 ) ) ;
#793 = ADVANCED_FACE ( 'NONE', ( #1018 ), #6391, .T. ) ;
#794 = AXIS2_PLACEMENT_3D ( 'NONE', #33, #7686, #6097 ) ;
#795 = CARTESIAN_POINT ( 'NONE',  ( 0.000000000000000000, 61.99999999999999289, 0.000000000000000000 ) ) ;
#796 = ORIENTED_EDGE ( 'NONE', *, *, #224, .F. ) ;
#797 = CARTESIAN_POINT ( 'NONE',  ( 9.984897811736454187, 3.936638391489574396, 41.37247550685020059 ) ) ;
#798 = ORIENTED_EDGE ( 'NONE', *, *, #1487, .T. ) ;
#799 = CARTESIAN_POINT ( 'NONE',  ( 5.371095444502685723, 60.99999999999999289, 34.07933880998929510 ) ) ;
#800 = CARTESIAN_POINT ( 'NONE',  ( 6.000000000000007994, -15.00000000000000000, 31.00000000000000711 ) ) ;
#801 = EDGE_LOOP ( 'NONE', ( #7375, #4405, #5867, #3569 ) ) ;
#802 = DIRECTION ( 'NONE',  ( -0.000000000000000000, 1.000000000000000000, -0.000000000000000000 ) ) ;
#803 = VECTOR ( 'NONE', #7890, 1000.000000000000000 ) ;
#804 = ORIENTED_EDGE ( 'NONE', *, *, #7649, .F. ) ;
#805 = CARTESIAN_POINT ( 'NONE',  ( 1.221566888952841201E-22, 27.99999999999992184, -31.00000000000000711 ) ) ;
#806 = B_SPLINE_CURVE_WITH_KNOTS ( 'NONE', 3,
 ( #9050, #9248, #6810, #1591 ),
 .UNSPECIFIED., .F., .F.,
 ( 4, 4 ),
 ( 0.000000000000000000, 0.001643226871903047392 ),
 .UNSPECIFIED. ) ;
#807 = CARTESIAN_POINT ( 'NONE',  ( 32.59762842694625817, 61.99999999999999289, -3.637569555611369854 ) ) ;
#808 = CARTESIAN_POINT ( 'NONE',  ( -7.945459518470957327, -2.812008134636945655, 42.35892031214973485 ) ) ;
#809 = AXIS2_PLACEMENT_3D ( 'NONE', #3438, #7888, #1997 ) ;
#810 = EDGE_CURVE ( 'NONE', #7824, #1842, #4038, .T. ) ;
#811 = ORIENTED_EDGE ( 'NONE', *, *, #6176, .T. ) ;
#812 = CARTESIAN_POINT ( 'NONE',  ( -5.775154784098236682, 58.97791112757357723, 35.56426808734908462 ) ) ;
#813 = ORIENTED_EDGE ( 'NONE', *, *, #5473, .F. ) ;
#814 = UNCERTAINTY_MEASURE_WITH_UNIT (LENGTH_MEASURE( 1.000000000000000082E-05 ), #3122, 'distance_accuracy_value', 'NONE');
#815 = EDGE_LOOP ( 'NONE', ( #247, #8601, #275, #4670 ) ) ;
#816 = AXIS2_PLACEMENT_3D ( 'NONE', #3083, #4481, #2339 ) ;
#817 = CARTESIAN_POINT ( 'NONE',  ( -2.621723037464307460, -6.360998902849781089, 43.82648660254912443 ) ) ;
#818 = ADVANCED_FACE ( 'NONE', ( #7842 ), #380, .T. ) ;
#819 = DIRECTION ( 'NONE',  ( -0.000000000000000000, -1.000000000000000000, -0.000000000000000000 ) ) ;
#820 = CARTESIAN_POINT ( 'NONE',  ( 5.562309845551833831, 59.00253480853272947, -35.56426808735054834 ) ) ;
#821 = EDGE_CURVE ( 'NONE', #9092, #667, #3230, .T. ) ;
#822 = ORIENTED_EDGE ( 'NONE', *, *, #1375, .F. ) ;
#823 = DIRECTION ( 'NONE',  ( 0.000000000000000000, 0.000000000000000000, 1.000000000000000000 ) ) ;
#824 = CARTESIAN_POINT ( 'NONE',  ( -5.999999999999998224, -10.00000000000000533, 26.32489316217636954 ) ) ;
#825 = EDGE_CURVE ( 'NONE', #7758, #8266, #9312, .T. ) ;
#826 = ORIENTED_EDGE ( 'NONE', *, *, #1722, .F. ) ;
#827 = CARTESIAN_POINT ( 'NONE',  ( 2.204364238465235033E-15, -50.91168824543140659, -17.99999999999999645 ) ) ;
#828 = AXIS2_PLACEMENT_3D ( 'NONE', #5685, #4218, #5543 ) ;
#829 = DIRECTION ( 'NONE',  ( -1.820952055660014662E-28, -1.000000000000000000, -7.038118388768679669E-30 ) ) ;
#830 = FACE_OUTER_BOUND ( 'NONE', #8162, .T. ) ;
#831 = EDGE_CURVE ( 'NONE', #6918, #8994, #969, .T. ) ;
#832 = DIRECTION ( 'NONE',  ( -0.000000000000000000, 1.000000000000000000, -0.000000000000000000 ) ) ;
#833 = SURFACE_STYLE_FILL_AREA ( #2235 ) ;
#834 = EDGE_CURVE ( 'NONE', #4792, #6355, #8574, .T. ) ;
#835 = LINE ( 'NONE', #3841, #4426 ) ;
#836 = ORIENTED_EDGE ( 'NONE', *, *, #6420, .T. ) ;
#837 = EDGE_CURVE ( 'NONE', #7858, #6645, #2417, .T. ) ;
#838 = DIRECTION ( 'NONE',  ( 0.000000000000000000, 0.000000000000000000, 1.000000000000000000 ) ) ;
#839 = EDGE_LOOP ( 'NONE', ( #6390, #5258, #3782, #4715, #3267 ) ) ;
#840 = FACE_OUTER_BOUND ( 'NONE', #8194, .T. ) ;
#841 = EDGE_LOOP ( 'NONE', ( #4909, #7923, #1571, #5597 ) ) ;
#842 = DIRECTION ( 'NONE',  ( -0.000000000000000000, 1.000000000000000000, -0.000000000000000000 ) ) ;
#843 = CARTESIAN_POINT ( 'NONE',  ( 0.8530757223511000742, -15.00000000000015987, 36.76494129545336875 ) ) ;
#844 = AXIS2_PLACEMENT_3D ( 'NONE', #1890, #1990, #1847 ) ;
#845 = CIRCLE ( 'NONE', #8729, 40.00000000000000711 ) ;
#846 = ORIENTED_EDGE ( 'NONE', *, *, #9159, .F. ) ;
#847 = CARTESIAN_POINT ( 'NONE',  ( -30.00000000000000711, 30.00000000000000000, 5.000000000000011546 ) ) ;
#848 = DIRECTION ( 'NONE',  ( 1.000000000000000000, 0.000000000000000000, 0.000000000000000000 ) ) ;
#849 = VERTEX_POINT ( 'NONE', #6339 ) ;
#850 = PRODUCT_DEFINITION ( 'UNKNOWN', '', #5853, #3314 ) ;
#851 = CARTESIAN_POINT ( 'NONE',  ( 8.889207912806641687, -1.327353063715156933, 38.12328956942888425 ) ) ;
#852 = ITEM_DEFINED_TRANSFORMATION ( 'NONE', 'NONE', #3004,  #6314 ) ;
#853 = ORIENTED_EDGE ( 'NONE', *, *, #1832, .F. ) ;
#854 = DIRECTION ( 'NONE',  ( -1.820952055660014662E-28, -1.000000000000000000, -7.038118388768679669E-30 ) ) ;
#855 = DIRECTION ( 'NONE',  ( 1.000000000000000000, 0.000000000000000000, 0.000000000000000000 ) ) ;
#856 = ORIENTED_EDGE ( 'NONE', *, *, #5980, .T. ) ;
#857 = CARTESIAN_POINT ( 'NONE',  ( 0.000000000000000000, 60.99999999999999289, 0.000000000000000000 ) ) ;
#858 = ORIENTED_EDGE ( 'NONE', *, *, #834, .F. ) ;
#859 = CARTESIAN_POINT ( 'NONE',  ( -9.866174171641793222, 4.958453368138042272, 41.43661138559432544 ) ) ;
#860 = PLANE ( 'NONE',  #9656 ) ;
#861 = DIRECTION ( 'NONE',  ( 0.000000000000000000, 0.000000000000000000, 1.000000000000000000 ) ) ;
#862 = VECTOR ( 'NONE', #2490, 1000.000000000000000 ) ;
#863 = ORIENTED_EDGE ( 'NONE', *, *, #1217, .F. ) ;
#864 = CARTESIAN_POINT ( 'NONE',  ( 32.85680095556730862, 59.99999999999999289, 3.070933240276029874 ) ) ;
#865 = ORIENTED_EDGE ( 'NONE', *, *, #1471, .F. ) ;
#866 = ORIENTED_EDGE ( 'NONE', *, *, #4695, .F. ) ;
#867 = CARTESIAN_POINT ( 'NONE',  ( -3.062418613096201447, -11.31009261275296218, 38.88193483011423268 ) ) ;
#868 = EDGE_CURVE ( 'NONE', #577, #2358, #6977, .T. ) ;
#869 = CARTESIAN_POINT ( 'NONE',  ( 1.300000000000000044, 3.252606517456513302E-16, 2.499999999999999556 ) ) ;
#870 = AXIS2_PLACEMENT_3D ( 'NONE', #3899, #2299, #4731 ) ;
#871 = AXIS2_PLACEMENT_3D ( 'NONE', #7357, #8885, #5724 ) ;
#872 = FACE_OUTER_BOUND ( 'NONE', #7624, .T. ) ;
#873 = PRODUCT_DEFINITION_SHAPE ( 'NONE', 'NONE',  #9760 ) ;
#874 = VERTEX_POINT ( 'NONE', #8631 ) ;
#875 = CARTESIAN_POINT ( 'NONE',  ( 3.796404955196288922E-15, 27.99999999999992184, 31.00000000000000711 ) ) ;
#876 = DIRECTION ( 'NONE',  ( -0.3271946967961539277, 0.000000000000000000, 0.9449569463147370341 ) ) ;
#877 = CIRCLE ( 'NONE', #6381, 33.00000000000000711 ) ;
#878 = CARTESIAN_POINT ( 'NONE',  ( -3.516611797194481248, 59.70849920474193340, 34.51129295977867883 ) ) ;
#879 = VECTOR ( 'NONE', #5666, 1000.000000000000114 ) ;
#880 = VERTEX_POINT ( 'NONE', #9420 ) ;
#881 = FACE_OUTER_BOUND ( 'NONE', #3150, .T. ) ;
#882 = CARTESIAN_POINT ( 'NONE',  ( 5.562309845534588959, 69.99999999999998579, -33.06426808735054124 ) ) ;
#883 = DIRECTION ( 'NONE',  ( -0.3286710990610922090, -6.289316826390952918E-29, -0.9444444444444435316 ) ) ;
#884 = DIRECTION ( 'NONE',  ( 0.000000000000000000, -0.000000000000000000, 1.000000000000000000 ) ) ;
#885 = ORIENTED_EDGE ( 'NONE', *, *, #5170, .T. ) ;
#886 = DIRECTION ( 'NONE',  ( -0.000000000000000000, 1.000000000000000000, -0.000000000000000000 ) ) ;
#887 = VECTOR ( 'NONE', #9049, 1000.000000000000000 ) ;
#888 = CIRCLE ( 'NONE', #8608, 27.00000000000000355 ) ;
#889 = EDGE_CURVE ( 'NONE', #7059, #4514, #9064, .T. ) ;
#890 = EDGE_CURVE ( 'NONE', #9115, #5960, #5703, .T. ) ;
#891 = ADVANCED_FACE ( 'NONE', ( #8075 ), #3481, .F. ) ;
#892 = VECTOR ( 'NONE', #8543, 1000.000000000000341 ) ;
#893 = VECTOR ( 'NONE', #2160, 1000.000000000000000 ) ;
#894 = DIRECTION ( 'NONE',  ( 0.000000000000000000, 0.000000000000000000, 1.000000000000000000 ) ) ;
#895 = ORIENTED_EDGE ( 'NONE', *, *, #4487, .F. ) ;
#896 = DIRECTION ( 'NONE',  ( 0.000000000000000000, 0.000000000000000000, 1.000000000000000000 ) ) ;
#897 = DIRECTION ( 'NONE',  ( -0.000000000000000000, 1.000000000000000000, -0.000000000000000000 ) ) ;
#898 = ORIENTED_EDGE ( 'NONE', *, *, #5824, .F. ) ;
#899 = DIRECTION ( 'NONE',  ( -1.000000000000000000, 0.000000000000000000, -1.047444401652940795E-14 ) ) ;
#900 = VECTOR ( 'NONE', #3307, 1000.000000000000000 ) ;
#901 = CARTESIAN_POINT ( 'NONE',  ( 33.06426808735054124, 69.99999999999998579, 8.062309845534588959 ) ) ;
#902 = CARTESIAN_POINT ( 'NONE',  ( 6.828744152548106960, -4.017693012958108767, 42.79257513738735241 ) ) ;
#903 = VERTEX_POINT ( 'NONE', #9505 ) ;
#904 = DIRECTION ( 'NONE',  ( -0.000000000000000000, 1.000000000000000000, -0.000000000000000000 ) ) ;
#905 = AXIS2_PLACEMENT_3D ( 'NONE', #6737, #5223, #7491 ) ;
#906 = LINE ( 'NONE', #1540, #8759 ) ;
#907 = ORIENTED_EDGE ( 'NONE', *, *, #4031, .F. ) ;
#908 = CARTESIAN_POINT ( 'NONE',  ( -28.34870838944214455, 59.99999999999999289, -9.815840903884556212 ) ) ;
#909 = VERTEX_POINT ( 'NONE', #5892 ) ;
#910 = DIRECTION ( 'NONE',  ( 0.000000000000000000, 0.000000000000000000, 1.000000000000000000 ) ) ;
#911 = DIRECTION ( 'NONE',  ( 0.6195972517514870548, -0.000000000000000000, 0.7849198975831892522 ) ) ;
#912 = ORIENTED_EDGE ( 'NONE', *, *, #1001, .T. ) ;
#913 = CARTESIAN_POINT ( 'NONE',  ( -5.512087641164731266, -8.278301759323600351, 38.98172623838953399 ) ) ;
#914 = ORIENTED_EDGE ( 'NONE', *, *, #2519, .F. ) ;
#915 = VERTEX_POINT ( 'NONE', #7983 ) ;
#916 = EDGE_CURVE ( 'NONE', #5506, #2973, #8028, .T. ) ;
#917 = CARTESIAN_POINT ( 'NONE',  ( -3.052805839235613661, -6.247915692633487339, 38.91814572147156781 ) ) ;
#918 = PLANE ( 'NONE',  #6689 ) ;
#919 = CARTESIAN_POINT ( 'NONE',  ( 0.000000000000000000, 59.99999999999999289, -33.00000000000000711 ) ) ;
#920 = EDGE_LOOP ( 'NONE', ( #8639, #3272, #4380, #5538 ) ) ;
#921 = DIRECTION ( 'NONE',  ( -0.000000000000000000, -1.000000000000000000, -0.000000000000000000 ) ) ;
#922 = EDGE_LOOP ( 'NONE', ( #3656, #1162 ) ) ;
#923 = DIRECTION ( 'NONE',  ( 1.820952055660014662E-28, 1.000000000000000000, -6.508102468073347395E-30 ) ) ;
#924 = CARTESIAN_POINT ( 'NONE',  ( 4.861949598180850707, 59.13521925290943670, -35.48792514263537612 ) ) ;
#925 = CARTESIAN_POINT ( 'NONE',  ( 28.37252191822216218, 30.00000000000000000, 6.000000000000000000 ) ) ;
#926 = CARTESIAN_POINT ( 'NONE',  ( 2.603483962722058287, 18.02285644508602402, 38.91836598778383660 ) ) ;
#927 = CARTESIAN_POINT ( 'NONE',  ( 0.000000000000000000, 30.99999999999998579, 0.000000000000000000 ) ) ;
#928 = VERTEX_POINT ( 'NONE', #8770 ) ;
#929 = LINE ( 'NONE', #1025, #9706 ) ;
#930 = EDGE_CURVE ( 'NONE', #7030, #7610, #9528, .T. ) ;
#931 = FACE_OUTER_BOUND ( 'NONE', #1919, .T. ) ;
#932 = EDGE_LOOP ( 'NONE', ( #6935, #6466, #9602, #8022, #6551 ) ) ;
#933 = LINE ( 'NONE', #3195, #5567 ) ;
#934 = CARTESIAN_POINT ( 'NONE',  ( 37.38678512219217254, 61.82631808411006347, 6.843790051325325585 ) ) ;
#935 = ORIENTED_EDGE ( 'NONE', *, *, #2688, .F. ) ;
#936 = ADVANCED_FACE ( 'NONE', ( #1944, #1219 ), #1896, .F. ) ;
#937 = EDGE_CURVE ( 'NONE', #1495, #1081, #5017, .T. ) ;
#938 = DIRECTION ( 'NONE',  ( 0.000000000000000000, 0.000000000000000000, 1.000000000000000000 ) ) ;
#939 = ADVANCED_FACE ( 'NONE', ( #1264 ), #9558, .T. ) ;
#940 = CARTESIAN_POINT ( 'NONE',  ( 1.300000000000000044, 0.000000000000000000, -1.250000000000000000 ) ) ;
#941 = EDGE_LOOP ( 'NONE', ( #8806, #3621, #640, #6708, #7358 ) ) ;
#942 = VECTOR ( 'NONE', #6726, 1000.000000000000000 ) ;
#943 = CARTESIAN_POINT ( 'NONE',  ( 0.8597079678303534145, -11.70708081913769050, 39.00058418212047684 ) ) ;
#944 = CARTESIAN_POINT ( 'NONE',  ( 0.000000000000000000, 60.99999999999999289, 0.000000000000000000 ) ) ;
#945 = ORIENTED_EDGE ( 'NONE', *, *, #8555, .F. ) ;
#946 = DIRECTION ( 'NONE',  ( -0.000000000000000000, 1.000000000000000000, -0.000000000000000000 ) ) ;
#947 = DIRECTION ( 'NONE',  ( 1.735493991486225692E-29, -6.508102468073347395E-30, -1.000000000000000000 ) ) ;
#948 = CARTESIAN_POINT ( 'NONE',  ( 30.00000000000000711, 30.00000000000000000, 5.000000000000000888 ) ) ;
#949 = ORIENTED_EDGE ( 'NONE', *, *, #7446, .F. ) ;
#950 = EDGE_CURVE ( 'NONE', #6089, #8994, #8820, .T. ) ;
#951 = VECTOR ( 'NONE', #5557, 1000.000000000000000 ) ;
#952 = EDGE_CURVE ( 'NONE', #3643, #6132, #8814, .T. ) ;
#953 = CARTESIAN_POINT ( 'NONE',  ( 25.51470164434615029, 30.00000000000000000, -5.000000000000007105 ) ) ;
#954 = CARTESIAN_POINT ( 'NONE',  ( -9.934621505046441925, 1.974978613517290427, 41.40018739529156022 ) ) ;
#955 = VECTOR ( 'NONE', #1121, 1000.000000000000000 ) ;
#956 = EDGE_LOOP ( 'NONE', ( #1913, #7125, #1447, #1645 ) ) ;
#957 = DIRECTION ( 'NONE',  ( 0.000000000000000000, 0.000000000000000000, -1.000000000000000000 ) ) ;
#958 = ORIENTED_EDGE ( 'NONE', *, *, #592, .T. ) ;
#959 = ORIENTED_EDGE ( 'NONE', *, *, #6232, .F. ) ;
#960 = VERTEX_POINT ( 'NONE', #7329 ) ;
#961 = CARTESIAN_POINT ( 'NONE',  ( -6.703682056317219029, -9.695813972231860589, 38.42653128846041000 ) ) ;
#962 = PRESENTATION_STYLE_ASSIGNMENT (( #8420 ) ) ;
#963 = AXIS2_PLACEMENT_3D ( 'NONE', #7215, #5645, #3508 ) ;
#964 = CARTESIAN_POINT ( 'NONE',  ( -33.06426808735054124, 49.99999999999999289, -5.562309845534581854 ) ) ;
#965 = EDGE_CURVE ( 'NONE', #2396, #1296, #7185, .T. ) ;
#966 = ORIENTED_EDGE ( 'NONE', *, *, #4720, .T. ) ;
#967 = PLANE ( 'NONE',  #794 ) ;
#968 = ORIENTED_EDGE ( 'NONE', *, *, #8427, .T. ) ;
#969 = LINE ( 'NONE', #2437, #5435 ) ;
#970 = CARTESIAN_POINT ( 'NONE',  ( 7.935670091272698734, 60.00000000000000711, -32.24976038726181571 ) ) ;
#971 = FACE_OUTER_BOUND ( 'NONE', #4525, .T. ) ;
#972 = SURFACE_STYLE_FILL_AREA ( #4782 ) ;
#973 = DIRECTION ( 'NONE',  ( -1.820952055660014662E-28, -1.000000000000000000, -7.038118388768679669E-30 ) ) ;
#974 = CARTESIAN_POINT ( 'NONE',  ( -27.56211685706797709, 60.99999999999999289, -15.25056439471436676 ) ) ;
#975 = CARTESIAN_POINT ( 'NONE',  ( 0.7189834692050188769, -15.00000000000000000, 30.52844133725295706 ) ) ;
#976 = AXIS2_PLACEMENT_3D ( 'NONE', #7526, #1546, #19 ) ;
#977 = AXIS2_PLACEMENT_3D ( 'NONE', #5178, #8186, #3741 ) ;
#978 = DIRECTION ( 'NONE',  ( -1.000000000000000000, -0.000000000000000000, -0.000000000000000000 ) ) ;
#979 = ORIENTED_EDGE ( 'NONE', *, *, #1214, .T. ) ;
#980 = CARTESIAN_POINT ( 'NONE',  ( -5.562309845534701758, 60.99999999999999289, 33.06426808735052703 ) ) ;
#981 = CARTESIAN_POINT ( 'NONE',  ( 37.56827137616963341, 61.82639507982414528, 5.763559184779289524 ) ) ;
#982 = VERTEX_POINT ( 'NONE', #3580 ) ;
#983 = EDGE_CURVE ( 'NONE', #1128, #427, #7232, .T. ) ;
#984 = AXIS2_PLACEMENT_3D ( 'NONE', #219, #6220, #2324 ) ;
#985 = CARTESIAN_POINT ( 'NONE',  ( -13.53485947486097984, 3.294852476641296768, 295.0000000000000000 ) ) ;
#986 = LINE ( 'NONE', #1768, #108 ) ;
#987 = VERTEX_POINT ( 'NONE', #5846 ) ;
#988 = EDGE_CURVE ( 'NONE', #1527, #1864, #4967, .T. ) ;
#989 = CARTESIAN_POINT ( 'NONE',  ( 1.902041552336364516, -6.533359847113549890, 38.97006628291147479 ) ) ;
#990 = CARTESIAN_POINT ( 'NONE',  ( -8.216777476527294510, 53.00000000000031974, -23.61111111111111427 ) ) ;
#991 = EDGE_CURVE ( 'NONE', #6002, #8252, #1567, .T. ) ;
#992 = CIRCLE ( 'NONE', #6347, 27.00000000000000355 ) ;
#993 = ORIENTED_EDGE ( 'NONE', *, *, #2276, .F. ) ;
#994 = CARTESIAN_POINT ( 'NONE',  ( -8.550110809860612449, 60.00000000000029843, -24.56895259980339929 ) ) ;
#995 = DIRECTION ( 'NONE',  ( 0.3286710990611269034, -0.000000000000000000, 0.9444444444444316522 ) ) ;
#996 = VERTEX_POINT ( 'NONE', #5804 ) ;
#997 = DIRECTION ( 'NONE',  ( -1.820952055660014662E-28, -1.000000000000000000, -7.038118388768679669E-30 ) ) ;
#998 = VECTOR ( 'NONE', #911, 1000.000000000000114 ) ;
#999 = CARTESIAN_POINT ( 'NONE',  ( -12.48950176432141923, 39.99999999999999289, -35.88888888888889284 ) ) ;
#1000 = EDGE_CURVE ( 'NONE', #7794, #6031, #8346, .T. ) ;
#1001 = EDGE_CURVE ( 'NONE', #8160, #1864, #7383, .T. ) ;
#1002 = EDGE_LOOP ( 'NONE', ( #5300, #5992, #7430, #4313 ) ) ;
#1003 = CARTESIAN_POINT ( 'NONE',  ( -35.21620900558183820, 59.09151583898437821, -6.845072491844675255 ) ) ;
#1004 = ADVANCED_FACE ( 'NONE', ( #620 ), #2038, .F. ) ;
#1005 = VERTEX_POINT ( 'NONE', #7661 ) ;
#1006 = CARTESIAN_POINT ( 'NONE',  ( 34.69710844949434403, 59.33700357310857498, 7.462191142828216606 ) ) ;
#1007 = ORIENTED_EDGE ( 'NONE', *, *, #3223, .T. ) ;
#1008 = VERTEX_POINT ( 'NONE', #8884 ) ;
#1009 = CARTESIAN_POINT ( 'NONE',  ( -8.134414903913882000, -8.580173454344276252, 38.14378512097410123 ) ) ;
#1010 = CARTESIAN_POINT ( 'NONE',  ( 0.000000000000000000, 54.99999999999999289, 0.000000000000000000 ) ) ;
#1011 = DIRECTION ( 'NONE',  ( -0.000000000000000000, 1.000000000000000000, -0.000000000000000000 ) ) ;
#1012 = EDGE_CURVE ( 'NONE', #6132, #8213, #638, .T. ) ;
#1013 = ORIENTED_EDGE ( 'NONE', *, *, #1538, .T. ) ;
#1014 = PLANE ( 'NONE',  #7423 ) ;
#1015 = AXIS2_PLACEMENT_3D ( 'NONE', #5064, #4381, #9466 ) ;
#1016 = AXIS2_PLACEMENT_3D ( 'NONE', #5940, #6582, #8962 ) ;
#1017 = VERTEX_POINT ( 'NONE', #6505 ) ;
#1018 = FACE_OUTER_BOUND ( 'NONE', #7000, .T. ) ;
#1019 = FACE_OUTER_BOUND ( 'NONE', #9246, .T. ) ;
#1020 = CARTESIAN_POINT ( 'NONE',  ( 10.00000000000001599, 3.294852476638864491, 41.36423575989288537 ) ) ;
#1021 = CIRCLE ( 'NONE', #1963, 33.00000000000000711 ) ;
#1022 =( NAMED_UNIT ( * ) SI_UNIT ( $, .STERADIAN. ) SOLID_ANGLE_UNIT ( ) );
#1023 = VECTOR ( 'NONE', #3636, 1000.000000000000000 ) ;
#1024 = DIRECTION ( 'NONE',  ( -0.000000000000000000, -1.000000000000000000, -0.000000000000000000 ) ) ;
#1025 = CARTESIAN_POINT ( 'NONE',  ( -8.216777476527274970, 78.08723716182652197, -23.61111111111111427 ) ) ;
#1026=STYLED_ITEM('',(#9771),#6272);
#1027 = LINE ( 'NONE', #9185, #3047 ) ;
#1028 = ORIENTED_EDGE ( 'NONE', *, *, #41, .F. ) ;
#1029 = CARTESIAN_POINT ( 'NONE',  ( -33.06426808735054124, 49.99999999999999289, -5.562309845534581854 ) ) ;
#1030 = CARTESIAN_POINT ( 'NONE',  ( 38.00000000000000711, 54.99999999999999289, 1.288922537256478387E-13 ) ) ;
#1031 = AXIS2_PLACEMENT_3D ( 'NONE', #425, #5648, #3423 ) ;
#1032 = ORIENTED_EDGE ( 'NONE', *, *, #4563, .F. ) ;
#1033 = AXIS2_PLACEMENT_3D ( 'NONE', #7668, #8998, #6121 ) ;
#1034 = CARTESIAN_POINT ( 'NONE',  ( -6.109228642973866918, 11.23818579777762139, 43.04298740074260365 ) ) ;
#1035 = DIRECTION ( 'NONE',  ( -0.000000000000000000, -1.000000000000000000, -0.000000000000000000 ) ) ;
#1036 = CARTESIAN_POINT ( 'NONE',  ( 0.000000000000000000, 59.99999999999999289, 0.000000000000000000 ) ) ;
#1037 = CIRCLE ( 'NONE', #7977, 40.00000000000000711 ) ;
#1038 = VECTOR ( 'NONE', #8996, 1000.000000000000341 ) ;
#1039 = CARTESIAN_POINT ( 'NONE',  ( 7.734310478464688110, -8.915650141914058580, 38.22714239730741070 ) ) ;
#1040 = CONTEXT_DEPENDENT_SHAPE_REPRESENTATION ( #5438, #4898 ) ;
#1041 = AXIS2_PLACEMENT_3D ( 'NONE', #3721, #2820, #5974 ) ;
#1042 = DIRECTION ( 'NONE',  ( 0.3271946967961528174, -0.000000000000000000, -0.9449569463147374782 ) ) ;
#1043 = ORIENTED_EDGE ( 'NONE', *, *, #3461, .F. ) ;
#1044 = DIRECTION ( 'NONE',  ( -1.820952055660014662E-28, -1.000000000000000000, -7.038118388768679669E-30 ) ) ;
#1045 = FACE_OUTER_BOUND ( 'NONE', #4412, .T. ) ;
#1046 = ORIENTED_EDGE ( 'NONE', *, *, #4987, .T. ) ;
#1047 = CIRCLE ( 'NONE', #9404, 40.00000000000000711 ) ;
#1048 = DIRECTION ( 'NONE',  ( 0.000000000000000000, 1.000000000000000000, 0.000000000000000000 ) ) ;
#1049 = FACE_OUTER_BOUND ( 'NONE', #4097, .T. ) ;
#1050 = VECTOR ( 'NONE', #7003, 1000.000000000000000 ) ;
#1051 = ORIENTED_EDGE ( 'NONE', *, *, #2670, .F. ) ;
#1052 = CARTESIAN_POINT ( 'NONE',  ( -33.06426808735054124, 59.99999999999999289, -8.062309845534585406 ) ) ;
#1053 = ORIENTED_EDGE ( 'NONE', *, *, #1905, .F. ) ;
#1054 = CARTESIAN_POINT ( 'NONE',  ( 33.39503079668222085, 59.82426665968211665, 8.062309845534590735 ) ) ;
#1055 = ORIENTED_EDGE ( 'NONE', *, *, #509, .T. ) ;
#1056 = EDGE_LOOP ( 'NONE', ( #554, #4946, #5055, #1032 ) ) ;
#1057 = CARTESIAN_POINT ( 'NONE',  ( -10.00116243144523231, 2.568931457825094355, 37.85849583813012487 ) ) ;
#1058 = ADVANCED_FACE ( 'NONE', ( #5031 ), #7403, .T. ) ;
#1059 = ADVANCED_FACE ( 'NONE', ( #5622 ), #1075, .F. ) ;
#1060 = CARTESIAN_POINT ( 'NONE',  ( 5.562309845534932684, 61.99999999999999289, -33.06426808735049150 ) ) ;
#1061 = EDGE_CURVE ( 'NONE', #5641, #1736, #225, .T. ) ;
#1062 = CARTESIAN_POINT ( 'NONE',  ( -30.18708036726492594, 61.99999999999999289, -16.70299909897287094 ) ) ;
#1063 = EDGE_LOOP ( 'NONE', ( #4155, #7732, #4121, #7579 ) ) ;
#1064 = DIRECTION ( 'NONE',  ( 0.000000000000000000, 0.000000000000000000, -1.000000000000000000 ) ) ;
#1065 = CARTESIAN_POINT ( 'NONE',  ( -3.106744199778896931, 59.95265069314689299, 33.56539760714087350 ) ) ;
#1066 = EDGE_LOOP ( 'NONE', ( #230, #5982, #5408, #2955 ) ) ;
#1067 = CARTESIAN_POINT ( 'NONE',  ( -34.07933880998930221, 60.99999999999999289, 5.371095444502539173 ) ) ;
#1068 = DIRECTION ( 'NONE',  ( 0.000000000000000000, 1.000000000000000000, 0.000000000000000000 ) ) ;
#1069 = DIRECTION ( 'NONE',  ( -0.000000000000000000, -1.000000000000000000, -0.000000000000000000 ) ) ;
#1070 = DIRECTION ( 'NONE',  ( 0.000000000000000000, 0.000000000000000000, -1.000000000000000000 ) ) ;
#1071 = EDGE_CURVE ( 'NONE', #1104, #8562, #9429, .T. ) ;
#1072 = DIRECTION ( 'NONE',  ( -0.000000000000000000, 1.000000000000000000, -0.000000000000000000 ) ) ;
#1073 = EDGE_CURVE ( 'NONE', #8597, #6324, #9168, .T. ) ;
#1074 = VERTEX_POINT ( 'NONE', #6985 ) ;
#1075 = PLANE ( 'NONE',  #4000 ) ;
#1076 = APPLICATION_CONTEXT ( 'automotive_design' ) ;
#1077 = DIRECTION ( 'NONE',  ( -1.820459017594251978E-28, -1.000000000000000000, 6.508102468073347395E-30 ) ) ;
#1078 = ORIENTED_EDGE ( 'NONE', *, *, #6544, .F. ) ;
#1079 = DIRECTION ( 'NONE',  ( 0.000000000000000000, 0.000000000000000000, 1.000000000000000000 ) ) ;
#1080 = CARTESIAN_POINT ( 'NONE',  ( -8.673617379884032514E-16, 0.000000000000000000, -4.000000000000002665 ) ) ;
#1081 = VERTEX_POINT ( 'NONE', #1716 ) ;
#1082 = CARTESIAN_POINT ( 'NONE',  ( -8.216777476527274970, 47.00000000000034106, -23.61111111111107519 ) ) ;
#1083 = CARTESIAN_POINT ( 'NONE',  ( 2.326828918379971365E-15, 0.000000000000000000, 19.00000000000000355 ) ) ;
#1084 = LINE ( 'NONE', #8592, #6385 ) ;
#1085 = CARTESIAN_POINT ( 'NONE',  ( 3.212268717265503337, -6.180893100220475667, 43.73795460093941756 ) ) ;
#1086 = ORIENTED_EDGE ( 'NONE', *, *, #668, .F. ) ;
#1087 = CARTESIAN_POINT ( 'NONE',  ( 0.000000000000000000, 0.000000000000000000, -40.00000000000000711 ) ) ;
#1088 = EDGE_CURVE ( 'NONE', #7168, #7878, #5669, .T. ) ;
#1089 = VERTEX_POINT ( 'NONE', #2538 ) ;
#1090 = CARTESIAN_POINT ( 'NONE',  ( 0.000000000000000000, 60.99999999999999289, 0.000000000000000000 ) ) ;
#1091 = CARTESIAN_POINT ( 'NONE',  ( 0.000000000000000000, 30.99999999999998579, 0.000000000000000000 ) ) ;
#1092 = ORIENTED_EDGE ( 'NONE', *, *, #6366, .T. ) ;
#1093 = ADVANCED_FACE ( 'NONE', ( #4837 ), #7852, .F. ) ;
#1094 = FACE_OUTER_BOUND ( 'NONE', #2624, .T. ) ;
#1095 = DIRECTION ( 'NONE',  ( -0.5000000000000044409, 1.060575238724903587E-16, -0.8660254037844360431 ) ) ;
#1096 = DIRECTION ( 'NONE',  ( -0.000000000000000000, -1.000000000000000000, -0.000000000000000000 ) ) ;
#1097 = VERTEX_POINT ( 'NONE', #7089 ) ;
#1098 = CARTESIAN_POINT ( 'NONE',  ( 0.000000000000000000, 30.00000000000000000, 0.000000000000000000 ) ) ;
#1099 = ORIENTED_EDGE ( 'NONE', *, *, #6311, .T. ) ;
#1100 = DIRECTION ( 'NONE',  ( 0.000000000000000000, 1.000000000000000000, -0.000000000000000000 ) ) ;
#1101 = VERTEX_POINT ( 'NONE', #3341 ) ;
#1102 = VECTOR ( 'NONE', #3641, 1000.000000000000000 ) ;
#1103 = AXIS2_PLACEMENT_3D ( 'NONE', #3382, #9423, #7133 ) ;
#1104 = VERTEX_POINT ( 'NONE', #389 ) ;
#1105 = AXIS2_PLACEMENT_3D ( 'NONE', #7741, #6051, #3943 ) ;
#1106 = CARTESIAN_POINT ( 'NONE',  ( -12.95718999772756952, -0.1032853105602432597, 36.78477091561097723 ) ) ;
#1107 = CARTESIAN_POINT ( 'NONE',  ( -4.275055404930308001, 60.00000000000029843, -25.29156885273883049 ) ) ;
#1108 = EDGE_CURVE ( 'NONE', #667, #2443, #4931, .T. ) ;
#1109 = DIRECTION ( 'NONE',  ( 0.000000000000000000, 0.000000000000000000, 1.000000000000000000 ) ) ;
#1110 = B_SPLINE_CURVE_WITH_KNOTS ( 'NONE', 3,
 ( #2960, #3153, #3758, #6751 ),
 .UNSPECIFIED., .F., .F.,
 ( 4, 4 ),
 ( 0.000000000000000000, 0.001643226871903046308 ),
 .UNSPECIFIED. ) ;
#1111 = AXIS2_PLACEMENT_3D ( 'NONE', #5469, #3177, #9220 ) ;
#1112 = PRODUCT_DEFINITION_SHAPE ( 'NONE', 'NONE',  #9754 ) ;
#1113 = ORIENTED_EDGE ( 'NONE', *, *, #9629, .F. ) ;
#1114 = CARTESIAN_POINT ( 'NONE',  ( 13.53485947486097984, 3.294852476641298544, 300.0000000000000000 ) ) ;
#1115 = CARTESIAN_POINT ( 'NONE',  ( -3.070933240276028542, 59.99999999999999289, 32.85680095556730862 ) ) ;
#1116 = EDGE_LOOP ( 'NONE', ( #4082, #7773, #9193 ) ) ;
#1117 = DIRECTION ( 'NONE',  ( -1.820952055660014662E-28, -1.000000000000000000, -7.038118388768679669E-30 ) ) ;
#1118 = ADVANCED_FACE ( 'NONE', ( #8265 ), #3822, .F. ) ;
#1119 = DIRECTION ( 'NONE',  ( -0.000000000000000000, 1.000000000000000000, -0.000000000000000000 ) ) ;
#1120 = CARTESIAN_POINT ( 'NONE',  ( -8.216777476527294510, 59.00000000000029843, -23.61111111111111427 ) ) ;
#1121 = DIRECTION ( 'NONE',  ( 1.735493991486225972E-29, -6.508102468073347395E-30, -1.000000000000000000 ) ) ;
#1122 = AXIS2_PLACEMENT_3D ( 'NONE', #6934, #3989, #884 ) ;
#1123 = CARTESIAN_POINT ( 'NONE',  ( 3.429011037612588487E-15, 61.99999999999999289, 27.99999999999999289 ) ) ;
#1124 = EDGE_CURVE ( 'NONE', #2244, #300, #8320, .T. ) ;
#1125 = CARTESIAN_POINT ( 'NONE',  ( 0.000000000000000000, 39.99999999999999289, 0.000000000000000000 ) ) ;
#1126 = EDGE_CURVE ( 'NONE', #5694, #5111, #7904, .T. ) ;
#1127 = ADVANCED_FACE ( 'NONE', ( #5189 ), #5237, .F. ) ;
#1128 = VERTEX_POINT ( 'NONE', #3703 ) ;
#1129 = LINE ( 'NONE', #4932, #3212 ) ;
#1130 = ORIENTED_EDGE ( 'NONE', *, *, #2017, .F. ) ;
#1131 = DIRECTION ( 'NONE',  ( -1.000000000000000000, 0.000000000000000000, -3.491481338843133355E-15 ) ) ;
#1132 = DIRECTION ( 'NONE',  ( -1.820952055660014662E-28, -1.000000000000000000, 6.508102468073347395E-30 ) ) ;
#1133 = ORIENTED_EDGE ( 'NONE', *, *, #1233, .F. ) ;
#1134 = LINE ( 'NONE', #4292, #1183 ) ;
#1135 = DIRECTION ( 'NONE',  ( -0.000000000000000000, -1.000000000000000000, -0.000000000000000000 ) ) ;
#1136 = B_SPLINE_CURVE_WITH_KNOTS ( 'NONE', 3,
 ( #7546, #5900, #4584, #8927, #37, #775, #3785, #7393, #7591, #2145 ),
 .UNSPECIFIED., .F., .F.,
 ( 4, 2, 2, 2, 4 ),
 ( 0.003057178249550608282, 0.004067793317122878408, 0.005078408384695147666, 0.006089023452267415190, 0.007099638519839682714 ),
 .UNSPECIFIED. ) ;
#1137 = CARTESIAN_POINT ( 'NONE',  ( -37.56827137616963341, 61.82639507982414528, -5.763559184779289524 ) ) ;
#1138 = CARTESIAN_POINT ( 'NONE',  ( 0.000000000000000000, 59.99999999999999289, -37.00000000000000711 ) ) ;
#1139 = VERTEX_POINT ( 'NONE', #2110 ) ;
#1140 = CARTESIAN_POINT ( 'NONE',  ( 0.000000000000000000, 60.99999999999999289, 0.000000000000000000 ) ) ;
#1141 = ORIENTED_EDGE ( 'NONE', *, *, #4794, .F. ) ;
#1142 = CARTESIAN_POINT ( 'NONE',  ( 32.37987785958423359, 59.99097422714241645, 7.973032508609962932 ) ) ;
#1143 = DIRECTION ( 'NONE',  ( -0.3286710990611269034, 0.000000000000000000, -0.9444444444444315412 ) ) ;
#1144 = AXIS2_PLACEMENT_3D ( 'NONE', #2062, #3604, #5187 ) ;
#1145 = ORIENTED_EDGE ( 'NONE', *, *, #9427, .T. ) ;
#1146 = DIRECTION ( 'NONE',  ( -1.820952055660014662E-28, -1.000000000000000000, -7.038118388768679669E-30 ) ) ;
#1147 = DIRECTION ( 'NONE',  ( -0.000000000000000000, 1.000000000000000000, -0.000000000000000000 ) ) ;
#1148 = PRODUCT_DEFINITION_CONTEXT ( 'detailed design', #709, 'design' ) ;
#1149 = AXIS2_PLACEMENT_3D ( 'NONE', #9329, #4885, #1915 ) ;
#1150 = ORIENTED_EDGE ( 'NONE', *, *, #9390, .T. ) ;
#1151 = ORIENTED_EDGE ( 'NONE', *, *, #2796, .T. ) ;
#1152 = CARTESIAN_POINT ( 'NONE',  ( -33.39503079668222085, 59.82426665968211665, -8.062309845534588959 ) ) ;
#1153 = ORIENTED_EDGE ( 'NONE', *, *, #2248, .F. ) ;
#1154 = CARTESIAN_POINT ( 'NONE',  ( -8.216777476527274970, 78.08723716182652197, -23.61111111111111427 ) ) ;
#1155 = ORIENTED_EDGE ( 'NONE', *, *, #3946, .F. ) ;
#1156 = ORIENTED_EDGE ( 'NONE', *, *, #6662, .T. ) ;
#1157 = CARTESIAN_POINT ( 'NONE',  ( -9.363418156690336502, -0.2310869320007213068, 41.69859845502092099 ) ) ;
#1158 = AXIS2_PLACEMENT_3D ( 'NONE', #6526, #525, #3520 ) ;
#1159 = AXIS2_PLACEMENT_3D ( 'NONE', #2694, #1911, #3593 ) ;
#1160 = CYLINDRICAL_SURFACE ( 'NONE', #7665, 30.00000000000000711 ) ;
#1161 = DIRECTION ( 'NONE',  ( 1.820952055660014662E-28, 1.000000000000000000, 7.038118388768679669E-30 ) ) ;
#1162 = ORIENTED_EDGE ( 'NONE', *, *, #7492, .F. ) ;
#1163 = CARTESIAN_POINT ( 'NONE',  ( 15.97678174684330799, 61.99999999999999289, -28.87459861216662205 ) ) ;
#1164 = ORIENTED_EDGE ( 'NONE', *, *, #2925, .F. ) ;
#1165 = CARTESIAN_POINT ( 'NONE',  ( 0.000000000000000000, 0.000000000000000000, 0.000000000000000000 ) ) ;
#1166 = B_SPLINE_CURVE_WITH_KNOTS ( 'NONE', 3,
 ( #2835, #6543, #2982, #4479 ),
 .UNSPECIFIED., .F., .F.,
 ( 4, 4 ),
 ( 0.000000000000000000, 0.001643226871903046308 ),
 .UNSPECIFIED. ) ;
#1167 = CARTESIAN_POINT ( 'NONE',  ( 0.000000000000000000, -15.00000000000000000, 0.000000000000000000 ) ) ;
#1168 = CARTESIAN_POINT ( 'NONE',  ( 11.39612023638420091, -4.438368553505347869, 37.29814521415754314 ) ) ;
#1169 = DIRECTION ( 'NONE',  ( -0.000000000000000000, 1.000000000000000000, -0.000000000000000000 ) ) ;
#1170 = CARTESIAN_POINT ( 'NONE',  ( -16.70299909897276081, 60.99999999999999289, 30.18708036726496857 ) ) ;
#1171 = ADVANCED_FACE ( 'NONE', ( #3655 ), #2901, .T. ) ;
#1172 = VECTOR ( 'NONE', #4829, 999.9999999999998863 ) ;
#1173 = ORIENTED_EDGE ( 'NONE', *, *, #3240, .T. ) ;
#1174 = VECTOR ( 'NONE', #5910, 1000.000000000000341 ) ;
#1175 = CARTESIAN_POINT ( 'NONE',  ( 7.933835403919273332, 9.390567006709300557, 42.36121793582603345 ) ) ;
#1176 = ORIENTED_EDGE ( 'NONE', *, *, #7005, .T. ) ;
#1177 = CARTESIAN_POINT ( 'NONE',  ( 7.824319130992849937E-27, 43.00000000000019895, 2.858080037470658006E-28 ) ) ;
#1178 = PLANE ( 'NONE',  #117 ) ;
#1179 = CARTESIAN_POINT ( 'NONE',  ( -9.168699364306950983, 14.24186408291268435, 37.91585989658146616 ) ) ;
#1180 = EDGE_CURVE ( 'NONE', #5073, #3751, #2510, .T. ) ;
#1181 = EDGE_CURVE ( 'NONE', #2714, #269, #5546, .T. ) ;
#1182 = CARTESIAN_POINT ( 'NONE',  ( 9.219811829770575476E-27, 40.00000000000014921, -37.00000000000000711 ) ) ;
#1183 = VECTOR ( 'NONE', #345, 1000.000000000000000 ) ;
#1184 = EDGE_CURVE ( 'NONE', #8659, #1276, #737, .T. ) ;
#1185 = AXIS2_PLACEMENT_3D ( 'NONE', #2056, #2101, #2651 ) ;
#1186 = ADVANCED_FACE ( 'NONE', ( #2768 ), #3846, .F. ) ;
#1187 = CARTESIAN_POINT ( 'NONE',  ( 4.999999999999815259, 19.99999999999990763, 20.00000000000019185 ) ) ;
#1188 = VECTOR ( 'NONE', #5184, 1000.000000000000000 ) ;
#1189 = VECTOR ( 'NONE', #7916, 1000.000000000000000 ) ;
#1190 = ORIENTED_EDGE ( 'NONE', *, *, #8776, .F. ) ;
#1191 = FACE_OUTER_BOUND ( 'NONE', #5726, .T. ) ;
#1192 = CARTESIAN_POINT ( 'NONE',  ( -5.838309802342690702, -8.139381478159863903, 38.91646265135313598 ) ) ;
#1193 = VERTEX_POINT ( 'NONE', #9320 ) ;
#1194 = DIRECTION ( 'NONE',  ( 0.3271946967961539277, 0.000000000000000000, -0.9449569463147370341 ) ) ;
#1195 = CONICAL_SURFACE ( 'NONE', #8930, 37.99999999999999289, 0.7853981633974447263 ) ;
#1196 = AXIS2_PLACEMENT_3D ( 'NONE', #8264, #3118, #2972 ) ;
#1197 = CARTESIAN_POINT ( 'NONE',  ( -12.16083066526040213, 78.08723716182652197, -34.94444444444459918 ) ) ;
#1198 = TOROIDAL_SURFACE ( 'NONE', #1669, 37.00000000000000711, 3.000000000000002665 ) ;
#1199 = CIRCLE ( 'NONE', #7202, 26.00000000000017408 ) ;
#1200 = CIRCLE ( 'NONE', #4675, 1.500000000000000888 ) ;
#1201 = CARTESIAN_POINT ( 'NONE',  ( 10.56568760240365457, 12.41321854688487214, 37.54259628649076319 ) ) ;
#1202 = DIRECTION ( 'NONE',  ( 0.000000000000000000, 0.000000000000000000, 1.000000000000000000 ) ) ;
#1203 = VERTEX_POINT ( 'NONE', #2536 ) ;
#1204 = LINE ( 'NONE', #4953, #2126 ) ;
#1205 = VECTOR ( 'NONE', #1593, 1000.000000000000000 ) ;
#1206 = ORIENTED_EDGE ( 'NONE', *, *, #5319, .F. ) ;
#1207 = CARTESIAN_POINT ( 'NONE',  ( 1.138917931912835794E-26, 56.00000000000030553, -25.00000000000000000 ) ) ;
#1208 = EDGE_LOOP ( 'NONE', ( #6379, #6956, #7718, #4930, #229 ) ) ;
#1209 = ORIENTED_EDGE ( 'NONE', *, *, #412, .T. ) ;
#1210 = CARTESIAN_POINT ( 'NONE',  ( -9.937482190456421449, 1.998597242238694838, 41.39862281978090408 ) ) ;
#1211 = CARTESIAN_POINT ( 'NONE',  ( 0.000000000000000000, 59.99999999999999289, 0.000000000000000000 ) ) ;
#1212 = DIRECTION ( 'NONE',  ( -1.820952055660014662E-28, -1.000000000000000000, -7.038118388768679669E-30 ) ) ;
#1213 = AXIS2_PLACEMENT_3D ( 'NONE', #7796, #3345, #2493 ) ;
#1214 = EDGE_CURVE ( 'NONE', #982, #6796, #5568, .T. ) ;
#1215 = ORIENTED_EDGE ( 'NONE', *, *, #6641, .T. ) ;
#1216 = DIRECTION ( 'NONE',  ( 0.000000000000000000, 0.000000000000000000, 1.000000000000000000 ) ) ;
#1217 = EDGE_CURVE ( 'NONE', #6796, #4952, #9568, .T. ) ;
#1218 = ORIENTED_EDGE ( 'NONE', *, *, #2424, .T. ) ;
#1219 = FACE_OUTER_BOUND ( 'NONE', #8915, .T. ) ;
#1220 = DIRECTION ( 'NONE',  ( 0.000000000000000000, -0.000000000000000000, -1.000000000000000000 ) ) ;
#1221 = CARTESIAN_POINT ( 'NONE',  ( 12.17954565146988699, 9.319135634659431844, 37.04959301261877869 ) ) ;
#1222 = DIRECTION ( 'NONE',  ( 0.000000000000000000, 1.000000000000000000, -0.000000000000000000 ) ) ;
#1223 = DIRECTION ( 'NONE',  ( 0.000000000000000000, 0.000000000000000000, -1.000000000000000000 ) ) ;
#1224 = CIRCLE ( 'NONE', #4519, 1.999999999999999556 ) ;
#1225 = ORIENTED_EDGE ( 'NONE', *, *, #7891, .F. ) ;
#1226 = CARTESIAN_POINT ( 'NONE',  ( -32.37987785958423359, 59.99097422714241645, -7.973032508609959379 ) ) ;
#1227 = CARTESIAN_POINT ( 'NONE',  ( 9.479273386569138538, 6.546693577225376259, 41.64111890186204334 ) ) ;
#1228 = ORIENTED_EDGE ( 'NONE', *, *, #3352, .F. ) ;
#1229 = CARTESIAN_POINT ( 'NONE',  ( 1.300000000000000044, 0.7216878364870328300, 1.250000000000000000 ) ) ;
#1230 = CARTESIAN_POINT ( 'NONE',  ( 1.000867273499158728E-26, 44.50000000000019185, -37.00000000000000711 ) ) ;
#1231 = DIRECTION ( 'NONE',  ( -0.1666666666666658525, -3.897465909857536228E-29, -0.9860132971832695770 ) ) ;
#1232 = CARTESIAN_POINT ( 'NONE',  ( 1.020767103194353487, -9.471900692527622567, 39.52815712443386076 ) ) ;
#1233 = EDGE_CURVE ( 'NONE', #7715, #4557, #1235, .T. ) ;
#1234 = ADVANCED_FACE ( 'NONE', ( #439 ), #4182, .F. ) ;
#1235 = B_SPLINE_CURVE_WITH_KNOTS ( 'NONE', 3,
 ( #5370, #7544, #2289, #3128, #3834, #8380, #3179, #3227, #878, #2388, #7029, #7840, #1065, #5701, #7230, #1115 ),
 .UNSPECIFIED., .F., .F.,
 ( 4, 2, 2, 2, 2, 2, 2, 4 ),
 ( 0.005084922178573568659, 0.006146119420698883951, 0.006676718041761538561, 0.007207316662824192303, 0.007737915283886846046, 0.008268513904949498922, 0.008799112526012153532, 0.009329711147074808142 ),
 .UNSPECIFIED. ) ;
#1236 = CARTESIAN_POINT ( 'NONE',  ( -33.06426808735054124, 60.99999999999999289, -10.06230984553459251 ) ) ;
#1237 = ADVANCED_FACE ( 'NONE', ( #3328 ), #2678, .F. ) ;
#1238 = VERTEX_POINT ( 'NONE', #8812 ) ;
#1239 = LINE ( 'NONE', #9623, #9208 ) ;
#1240 = CARTESIAN_POINT ( 'NONE',  ( -0.8899638032320900116, -15.00000000000000000, 36.76490800571937712 ) ) ;
#1241 = EDGE_CURVE ( 'NONE', #7328, #5641, #699, .T. ) ;
#1242 = ORIENTED_EDGE ( 'NONE', *, *, #9562, .F. ) ;
#1243 = DIRECTION ( 'NONE',  ( -1.000000000000000000, -8.673617379884034239E-17, 0.000000000000000000 ) ) ;
#1244 = DIRECTION ( 'NONE',  ( -0.000000000000000000, 1.000000000000000000, -0.000000000000000000 ) ) ;
#1245 = CARTESIAN_POINT ( 'NONE',  ( 1.332947368826647772, 13.21112352634868792, 43.95731769652755361 ) ) ;
#1246 = EDGE_CURVE ( 'NONE', #4542, #9236, #5207, .T. ) ;
#1247 = ORIENTED_EDGE ( 'NONE', *, *, #6944, .T. ) ;
#1248 = DIRECTION ( 'NONE',  ( 0.000000000000000000, 0.000000000000000000, 1.000000000000000000 ) ) ;
#1249 = EDGE_CURVE ( 'NONE', #928, #9118, #4279, .T. ) ;
#1250 = ORIENTED_EDGE ( 'NONE', *, *, #6050, .T. ) ;
#1251 = CARTESIAN_POINT ( 'NONE',  ( 34.19425402209839859, 59.81545713833158828, 3.326151553796978355 ) ) ;
#1252 = VERTEX_POINT ( 'NONE', #618 ) ;
#1253 = EDGE_LOOP ( 'NONE', ( #2425, #643, #8630, #4172 ) ) ;
#1254 = ADVANCED_FACE ( 'NONE', ( #7431 ), #5844, .F. ) ;
#1255 = CARTESIAN_POINT ( 'NONE',  ( -3.222268259786776667, 12.78388326438595257, 43.74320717588041418 ) ) ;
#1256 = ADVANCED_FACE ( 'NONE', ( #3522 ), #7434, .T. ) ;
#1257 = CARTESIAN_POINT ( 'NONE',  ( 4.776122516674679455E-15, -4.999999999999997335, -39.00000000000002132 ) ) ;
#1258 = CARTESIAN_POINT ( 'NONE',  ( -5.999999999999998224, 30.00000000000000000, 28.37252191822216218 ) ) ;
#1259 = VECTOR ( 'NONE', #7731, 1000.000000000000000 ) ;
#1260 = AXIS2_PLACEMENT_3D ( 'NONE', #2829, #4137, #4282 ) ;
#1261 = ORIENTED_EDGE ( 'NONE', *, *, #7038, .F. ) ;
#1262 = LINE ( 'NONE', #9502, #4913 ) ;
#1263 = VERTEX_POINT ( 'NONE', #5939 ) ;
#1264 = FACE_OUTER_BOUND ( 'NONE', #1066, .T. ) ;
#1265 = DIRECTION ( 'NONE',  ( -1.047444401652940795E-14, -0.000000000000000000, 1.000000000000000000 ) ) ;
#1266 = CARTESIAN_POINT ( 'NONE',  ( 9.573718945232185362, 13.70885271580617371, 37.80730753525386945 ) ) ;
#1267 = DIRECTION ( 'NONE',  ( 0.000000000000000000, 0.000000000000000000, -1.000000000000000000 ) ) ;
#1268 = CARTESIAN_POINT ( 'NONE',  ( 0.000000000000000000, 3.294852476641296768, 184.6745183374407020 ) ) ;
#1269 = AXIS2_PLACEMENT_3D ( 'NONE', #7980, #1851, #9267 ) ;
#1270 = ADVANCED_BREP_SHAPE_REPRESENTATION ( '', ( #9647, #6314 ), #188 ) ;
#1271 = ADVANCED_FACE ( 'NONE', ( #4421 ), #3672, .F. ) ;
#1272 = ORIENTED_EDGE ( 'NONE', *, *, #8570, .F. ) ;
#1273 = DIRECTION ( 'NONE',  ( -1.000000000000000000, 0.000000000000000000, 0.000000000000000000 ) ) ;
#1274 = VECTOR ( 'NONE', #1169, 1000.000000000000000 ) ;
#1275 = DIRECTION ( 'NONE',  ( 1.735493991486225972E-29, -6.508102468073347395E-30, -1.000000000000000000 ) ) ;
#1276 = VERTEX_POINT ( 'NONE', #5015 ) ;
#1277 = DIRECTION ( 'NONE',  ( -0.000000000000000000, 1.000000000000000000, -0.000000000000000000 ) ) ;
#1278 = SURFACE_SIDE_STYLE ('',( #5859 ) ) ;
#1279 = FACE_OUTER_BOUND ( 'NONE', #2037, .T. ) ;
#1280 = DIRECTION ( 'NONE',  ( -1.820952055660014662E-28, -1.000000000000000000, -7.038118388768679669E-30 ) ) ;
#1281 = VECTOR ( 'NONE', #2735, 1000.000000000000000 ) ;
#1282 = DIRECTION ( 'NONE',  ( -1.084202172485503448E-16, 0.000000000000000000, -1.000000000000000000 ) ) ;
#1283 = DIRECTION ( 'NONE',  ( 0.000000000000000000, 0.000000000000000000, 1.000000000000000000 ) ) ;
#1284 = VECTOR ( 'NONE', #7130, 1000.000000000000000 ) ;
#1285 = ORIENTED_EDGE ( 'NONE', *, *, #4759, .T. ) ;
#1286 = CYLINDRICAL_SURFACE ( 'NONE', #3506, 30.00000000000000711 ) ;
#1287 = CARTESIAN_POINT ( 'NONE',  ( -1.713217124479214482, -14.99999999999999822, 36.76766103293256549 ) ) ;
#1288 = EDGE_CURVE ( 'NONE', #6115, #7606, #1262, .T. ) ;
#1289 = ORIENTED_EDGE ( 'NONE', *, *, #290, .F. ) ;
#1290 = DIRECTION ( 'NONE',  ( -0.9860132971832693549, -1.788557213313974126E-28, 0.1666666666666657970 ) ) ;
#1291 = DIRECTION ( 'NONE',  ( 1.735493991486225972E-29, -6.508102468073347395E-30, -1.000000000000000000 ) ) ;
#1292 = CARTESIAN_POINT ( 'NONE',  ( 7.946841957352148711, 9.373763190100603993, 42.35574965673851722 ) ) ;
#1293 = VECTOR ( 'NONE', #1382, 1000.000000000000000 ) ;
#1294 = EDGE_LOOP ( 'NONE', ( #2608, #6117, #2414, #6412, #3983, #3371, #3119, #4801, #2703, #6790, #7872, #215, #3801, #1055, #8486, #3710 ) ) ;
#1295 = CARTESIAN_POINT ( 'NONE',  ( 0.000000000000000000, 61.99999999999999289, -27.99999999999999289 ) ) ;
#1296 = VERTEX_POINT ( 'NONE', #578 ) ;
#1297 = CARTESIAN_POINT ( 'NONE',  ( 10.00000000000001599, 3.294852476641296768, 300.0000000000000000 ) ) ;
#1298 = ORIENTED_EDGE ( 'NONE', *, *, #4743, .F. ) ;
#1299 = PLANE ( 'NONE',  #6702 ) ;
#1300 = ORIENTED_EDGE ( 'NONE', *, *, #4920, .F. ) ;
#1301 = CARTESIAN_POINT ( 'NONE',  ( -7.505748137593764469, 9.946373970317027968, 38.40043516335172313 ) ) ;
#1302 = DIRECTION ( 'NONE',  ( 0.000000000000000000, 0.000000000000000000, 1.000000000000000000 ) ) ;
#1303 = AXIS2_PLACEMENT_3D ( 'NONE', #6185, #4630, #9308 ) ;
#1304 = LINE ( 'NONE', #8958, #5871 ) ;
#1305 = EDGE_CURVE ( 'NONE', #7141, #1519, #8622, .T. ) ;
#1306 = ADVANCED_FACE ( 'NONE', ( #1357 ), #7276, .F. ) ;
#1307 = EDGE_CURVE ( 'NONE', #3216, #9419, #3578, .T. ) ;
#1308 = ORIENTED_EDGE ( 'NONE', *, *, #6948, .F. ) ;
#1309 = CARTESIAN_POINT ( 'NONE',  ( 0.000000000000000000, 39.99999999999999289, 0.000000000000000000 ) ) ;
#1310 = ORIENTED_EDGE ( 'NONE', *, *, #2619, .F. ) ;
#1311 = ORIENTED_EDGE ( 'NONE', *, *, #3040, .T. ) ;
#1312 = DIRECTION ( 'NONE',  ( -1.735493991486225972E-29, 6.508102468073347395E-30, 1.000000000000000000 ) ) ;
#1313 = TOROIDAL_SURFACE ( 'NONE', #220, 33.00000000000000711, 5.000000000000000000 ) ;
#1314 = CARTESIAN_POINT ( 'NONE',  ( -8.545448575588366680, 59.00000000000029843, -24.55555555555556424 ) ) ;
#1315 = CARTESIAN_POINT ( 'NONE',  ( 12.79072861028647168, -0.8504798754438103181, 36.84338291468104387 ) ) ;
#1316 = FACE_OUTER_BOUND ( 'NONE', #2423, .T. ) ;
#1317 = DIRECTION ( 'NONE',  ( -0.000000000000000000, 1.000000000000000000, -0.000000000000000000 ) ) ;
#1318 = AXIS2_PLACEMENT_3D ( 'NONE', #3163, #4618, #861 ) ;
#1319 = LINE ( 'NONE', #5173, #4592 ) ;
#1320 = ORIENTED_EDGE ( 'NONE', *, *, #2371, .F. ) ;
#1321 = CYLINDRICAL_SURFACE ( 'NONE', #4674, 25.00000000000000000 ) ;
#1322 = CARTESIAN_POINT ( 'NONE',  ( 4.473343921463067474, 12.24450654772725855, 43.48755112989530147 ) ) ;
#1323 = ORIENTED_EDGE ( 'NONE', *, *, #3240, .F. ) ;
#1324 = CARTESIAN_POINT ( 'NONE',  ( 1.820000000000000062, 4.653657836759941744E-16, -3.799999999999999378 ) ) ;
#1325 = DIRECTION ( 'NONE',  ( -1.000000000000000000, -1.821691612758658688E-28, -1.735493991486225972E-29 ) ) ;
#1326 = DIRECTION ( 'NONE',  ( 1.820952055660014662E-28, 1.000000000000000000, 7.038118388768679669E-30 ) ) ;
#1327 = VECTOR ( 'NONE', #3797, 1000.000000000000000 ) ;
#1328 = CARTESIAN_POINT ( 'NONE',  ( 0.000000000000000000, 30.99999999999998579, 0.000000000000000000 ) ) ;
#1329 = ORIENTED_EDGE ( 'NONE', *, *, #2926, .F. ) ;
#1330 = DIRECTION ( 'NONE',  ( 0.000000000000000000, 0.000000000000000000, 1.000000000000000000 ) ) ;
#1331 = CARTESIAN_POINT ( 'NONE',  ( -0.7293704418356496966, -15.00000000000000000, 30.52676338768143083 ) ) ;
#1332 = ORIENTED_EDGE ( 'NONE', *, *, #1217, .T. ) ;
#1333 = CIRCLE ( 'NONE', #398, 2.199999999999999734 ) ;
#1334 = CARTESIAN_POINT ( 'NONE',  ( 0.000000000000000000, 39.99999999999999289, 0.000000000000000000 ) ) ;
#1335 = DIRECTION ( 'NONE',  ( 0.000000000000000000, 1.000000000000000000, 0.000000000000000000 ) ) ;
#1336 = DIRECTION ( 'NONE',  ( -1.820952055660014662E-28, -1.000000000000000000, -7.038118388768679669E-30 ) ) ;
#1337 = ORIENTED_EDGE ( 'NONE', *, *, #7754, .F. ) ;
#1338 = CARTESIAN_POINT ( 'NONE',  ( 7.755618280887227378, 9.651396785365637498, 38.35455593997478729 ) ) ;
#1339 = AXIS2_PLACEMENT_3D ( 'NONE', #1090, #6316, #9337 ) ;
#1340 = AXIS2_PLACEMENT_3D ( 'NONE', #8032, #8636, #2686 ) ;
#1341 = ORIENTED_EDGE ( 'NONE', *, *, #9122, .T. ) ;
#1342 = CARTESIAN_POINT ( 'NONE',  ( 12.48950176432140680, 54.99999999999999289, 35.88888888888889284 ) ) ;
#1343 = ORIENTED_EDGE ( 'NONE', *, *, #8556, .T. ) ;
#1344 = CARTESIAN_POINT ( 'NONE',  ( 0.000000000000000000, 39.99999999999999289, 0.000000000000000000 ) ) ;
#1345 = VERTEX_POINT ( 'NONE', #4379 ) ;
#1346 = FACE_OUTER_BOUND ( 'NONE', #518, .T. ) ;
#1347 = ORIENTED_EDGE ( 'NONE', *, *, #1633, .T. ) ;
#1348 = VECTOR ( 'NONE', #2407, 1000.000000000000000 ) ;
#1349 = CARTESIAN_POINT ( 'NONE',  ( -5.501707247662611877, 11.70083553198481319, 38.70428226897013957 ) ) ;
#1350 = AXIS2_PLACEMENT_3D ( 'NONE', #2273, #5311, #1644 ) ;
#1351 = VECTOR ( 'NONE', #678, 1000.000000000000000 ) ;
#1352 = CARTESIAN_POINT ( 'NONE',  ( -29.00000000000000355, 0.000000000000000000, -3.999999999999996447 ) ) ;
#1353 = AXIS2_PLACEMENT_3D ( 'NONE', #3373, #4912, #4229 ) ;
#1354 = DIRECTION ( 'NONE',  ( 0.000000000000000000, -1.000000000000000000, 0.000000000000000000 ) ) ;
#1355 = AXIS2_PLACEMENT_3D ( 'NONE', #2964, #6755, #1440 ) ;
#1356 = VERTEX_POINT ( 'NONE', #8072 ) ;
#1357 = FACE_OUTER_BOUND ( 'NONE', #4149, .T. ) ;
#1358 = VERTEX_POINT ( 'NONE', #3478 ) ;
#1359 = DIRECTION ( 'NONE',  ( 1.735493991486224571E-29, 0.000000000000000000, -1.000000000000000000 ) ) ;
#1360 = EDGE_CURVE ( 'NONE', #3751, #9075, #4593, .T. ) ;
#1361 = LINE ( 'NONE', #4475, #3620 ) ;
#1362 = DIRECTION ( 'NONE',  ( 0.000000000000000000, 0.000000000000000000, 1.000000000000000000 ) ) ;
#1363 = ADVANCED_FACE ( 'NONE', ( #6530 ), #8289, .F. ) ;
#1364 = CARTESIAN_POINT ( 'NONE',  ( 0.000000000000000000, -0.7216878364870318308, 1.250000000000000000 ) ) ;
#1365 = AXIS2_PLACEMENT_3D ( 'NONE', #7053, #995, #9202 ) ;
#1366 = CARTESIAN_POINT ( 'NONE',  ( 5.562309845534588959, 69.99999999999998579, -35.56426808735054834 ) ) ;
#1367 = CIRCLE ( 'NONE', #6878, 2.500000000000002220 ) ;
#1368 = ORIENTED_EDGE ( 'NONE', *, *, #7402, .F. ) ;
#1369 = DIRECTION ( 'NONE',  ( 0.000000000000000000, 1.000000000000000000, 0.000000000000000000 ) ) ;
#1370 = PLANE ( 'NONE',  #418 ) ;
#1371 = DIRECTION ( 'NONE',  ( 0.000000000000000000, 1.000000000000000000, 0.000000000000000000 ) ) ;
#1372 = EDGE_CURVE ( 'NONE', #9687, #5003, #1993, .T. ) ;
#1373 = DIRECTION ( 'NONE',  ( -1.000000000000000000, 0.000000000000000000, 0.000000000000000000 ) ) ;
#1374 = DIRECTION ( 'NONE',  ( 0.000000000000000000, -1.000000000000000000, 0.000000000000000000 ) ) ;
#1375 = EDGE_CURVE ( 'NONE', #3666, #996, #2781, .T. ) ;
#1376 = DIRECTION ( 'NONE',  ( -1.000000000000000000, -0.000000000000000000, -0.000000000000000000 ) ) ;
#1377 = DIRECTION ( 'NONE',  ( -0.000000000000000000, -1.000000000000000000, -0.000000000000000000 ) ) ;
#1378 = ORIENTED_EDGE ( 'NONE', *, *, #5490, .F. ) ;
#1379 = CARTESIAN_POINT ( 'NONE',  ( 0.02451486836956002016, 18.29482697815588566, 38.99999229514322252 ) ) ;
#1380 = CARTESIAN_POINT ( 'NONE',  ( -33.06426808735054124, 59.99999999999999289, -5.562309845534581854 ) ) ;
#1381 = VERTEX_POINT ( 'NONE', #2170 ) ;
#1382 = DIRECTION ( 'NONE',  ( -1.820952055660014662E-28, -1.000000000000000000, -7.038118388768679669E-30 ) ) ;
#1383 = DIRECTION ( 'NONE',  ( 0.000000000000000000, 0.000000000000000000, -1.000000000000000000 ) ) ;
#1384 = EDGE_LOOP ( 'NONE', ( #2181, #2570, #7626, #8864 ) ) ;
#1385 = B_SPLINE_CURVE_WITH_KNOTS ( 'NONE', 3,
 ( #2336, #1510, #4633, #1560 ),
 .UNSPECIFIED., .F., .F.,
 ( 4, 4 ),
 ( 0.009125339089286721786, 0.009329711147074794264 ),
 .UNSPECIFIED. ) ;
#1386 = EDGE_CURVE ( 'NONE', #3246, #2405, #6540, .T. ) ;
#1387 = CARTESIAN_POINT ( 'NONE',  ( 8.139368704184242631, 9.113401726372073242, 42.27313584737455443 ) ) ;
#1388 = ORIENTED_EDGE ( 'NONE', *, *, #9343, .F. ) ;
#1389 = CARTESIAN_POINT ( 'NONE',  ( -35.43299232931641995, 59.17741350630852537, -4.746722514775166601 ) ) ;
#1390 = ORIENTED_EDGE ( 'NONE', *, *, #1902, .F. ) ;
#1391 = CARTESIAN_POINT ( 'NONE',  ( 0.000000000000000000, 59.99999999999999289, 0.000000000000000000 ) ) ;
#1392 = EDGE_LOOP ( 'NONE', ( #772, #8170, #5356, #7756, #5921 ) ) ;
#1393 = CARTESIAN_POINT ( 'NONE',  ( 5.423418723394456162E-28, -2.066522830327504070E-28, -26.00000000000009592 ) ) ;
#1394 = APPLICATION_CONTEXT ( 'automotive_design' ) ;
#1395 = EDGE_LOOP ( 'NONE', ( #7967, #2318, #966, #609 ) ) ;
#1396 = CARTESIAN_POINT ( 'NONE',  ( -10.53299942811007917, 12.46136332956525905, 37.55180211538850443 ) ) ;
#1397 = DIRECTION ( 'NONE',  ( 1.735493991486227373E-29, 0.000000000000000000, -1.000000000000000000 ) ) ;
#1398 = LINE ( 'NONE', #7427, #3196 ) ;
#1399 = ORIENTED_EDGE ( 'NONE', *, *, #1725, .T. ) ;
#1400 = DIRECTION ( 'NONE',  ( 0.000000000000000000, 0.000000000000000000, -1.000000000000000000 ) ) ;
#1401 = ORIENTED_EDGE ( 'NONE', *, *, #6490, .F. ) ;
#1402 = LINE ( 'NONE', #3020, #5521 ) ;
#1403 = FACE_OUTER_BOUND ( 'NONE', #5650, .T. ) ;
#1404 = ADVANCED_FACE ( 'NONE', ( #3622 ), #8811, .T. ) ;
#1405 = DIRECTION ( 'NONE',  ( -0.000000000000000000, 1.000000000000000000, -0.000000000000000000 ) ) ;
#1406 = CONICAL_SURFACE ( 'NONE', #160, 1732.050807568856271, 1.047197551196592524 ) ;
#1407 = EDGE_CURVE ( 'NONE', #6987, #2912, #2825, .T. ) ;
#1408 = DIRECTION ( 'NONE',  ( 0.000000000000000000, 0.000000000000000000, 1.000000000000000000 ) ) ;
#1409 = VERTEX_POINT ( 'NONE', #8914 ) ;
#1410 = LINE ( 'NONE', #4431, #3241 ) ;
#1411 = DIRECTION ( 'NONE',  ( 1.735493991486225972E-29, -6.508102468073347395E-30, -1.000000000000000000 ) ) ;
#1412 = CARTESIAN_POINT ( 'NONE',  ( -34.07933880998930221, 61.99999999999999289, 5.371095444502539173 ) ) ;
#1413 = DIRECTION ( 'NONE',  ( -1.000000000000000000, 0.000000000000000000, -0.000000000000000000 ) ) ;
#1414 = CARTESIAN_POINT ( 'NONE',  ( 2.400000000000000799, 0.000000000000000000, 2.199999999999999734 ) ) ;
#1415 = AXIS2_PLACEMENT_3D ( 'NONE', #2262, #5296, #4611 ) ;
#1416 = CIRCLE ( 'NONE', #7249, 38.00000000000000711 ) ;
#1417 = CARTESIAN_POINT ( 'NONE',  ( -31.00000000000000711, 27.42469319230601243, -5.999999999999996447 ) ) ;
#1418 = EDGE_CURVE ( 'NONE', #1760, #8960, #8774, .T. ) ;
#1419 = ADVANCED_FACE ( 'NONE', ( #5456 ), #4671, .F. ) ;
#1420 = AXIS2_PLACEMENT_3D ( 'NONE', #332, #9364, #7235 ) ;
#1421 = EDGE_CURVE ( 'NONE', #1969, #3718, #6693, .T. ) ;
#1422 = CARTESIAN_POINT ( 'NONE',  ( 31.00000000000001066, 28.00044749928606791, -0.9877776005181261310 ) ) ;
#1423 = ORIENTED_EDGE ( 'NONE', *, *, #5719, .T. ) ;
#1424 = DIRECTION ( 'NONE',  ( 0.000000000000000000, -1.000000000000000000, 0.000000000000000000 ) ) ;
#1425 = EDGE_LOOP ( 'NONE', ( #811, #2910, #8328, #5890, #5870 ) ) ;
#1426 = CARTESIAN_POINT ( 'NONE',  ( -18.58791755254457456, 59.99999999999999289, -23.54759692749571443 ) ) ;
#1427 = CARTESIAN_POINT ( 'NONE',  ( 0.7189834697752452985, -15.00000000000000000, 30.52844133987663611 ) ) ;
#1428 = EDGE_LOOP ( 'NONE', ( #3995, #9372, #9203, #5540, #5218, #9162, #751, #1113, #6522, #9139, #8470, #7506 ) ) ;
#1429 = CIRCLE ( 'NONE', #8212, 30.00000000000000711 ) ;
#1430 = CARTESIAN_POINT ( 'NONE',  ( 0.000000000000000000, 39.99999999999999289, 0.000000000000000000 ) ) ;
#1431 = CYLINDRICAL_SURFACE ( 'NONE', #414, 1.999999999999999556 ) ;
#1432 = VERTEX_POINT ( 'NONE', #3874 ) ;
#1433 = ADVANCED_FACE ( 'NONE', ( #6917 ), #3769, .F. ) ;
#1434 = CARTESIAN_POINT ( 'NONE',  ( 9.994974281626689105, -6.644405053951256690, 37.70273452987021301 ) ) ;
#1435 = EDGE_LOOP ( 'NONE', ( #8983, #8517, #7630, #6035 ) ) ;
#1436 = DIRECTION ( 'NONE',  ( 0.000000000000000000, -1.000000000000000000, 0.000000000000000000 ) ) ;
#1437 = VERTEX_POINT ( 'NONE', #5979 ) ;
#1438 = CARTESIAN_POINT ( 'NONE',  ( 35.03233509200964590, 59.17868483491578502, 7.112484670352360538 ) ) ;
#1439 = ORIENTED_EDGE ( 'NONE', *, *, #6960, .F. ) ;
#1440 = DIRECTION ( 'NONE',  ( 0.000000000000000000, -0.000000000000000000, 1.000000000000000000 ) ) ;
#1441 = ORIENTED_EDGE ( 'NONE', *, *, #4415, .F. ) ;
#1442 = CARTESIAN_POINT ( 'NONE',  ( -0.6382276400259029314, 13.27990715202770566, 43.99233959860035981 ) ) ;
#1443 = PRODUCT_RELATED_PRODUCT_CATEGORY ( 'part', '', ( #3868 ) ) ;
#1444 = CARTESIAN_POINT ( 'NONE',  ( -33.06426808735054124, 60.99999999999999289, -3.062309845534580077 ) ) ;
#1445 = CARTESIAN_POINT ( 'NONE',  ( 0.000000000000000000, 1.000000000000014655, 0.000000000000000000 ) ) ;
#1446 = TOROIDAL_SURFACE ( 'NONE', #4772, 13.53485947486097984, 5.000000000000000000 ) ;
#1447 = ORIENTED_EDGE ( 'NONE', *, *, #9031, .T. ) ;
#1448 = CARTESIAN_POINT ( 'NONE',  ( -11.07761026121387538, -4.999999999999996447, 37.39366993089406321 ) ) ;
#1449 = ORIENTED_EDGE ( 'NONE', *, *, #8908, .F. ) ;
#1450 = DIRECTION ( 'NONE',  ( 0.000000000000000000, 0.000000000000000000, -1.000000000000000000 ) ) ;
#1451 = CYLINDRICAL_SURFACE ( 'NONE', #9001, 26.00000000000000355 ) ;
#1452 = AXIS2_PLACEMENT_3D ( 'NONE', #5249, #8260, #4518 ) ;
#1453 = DIRECTION ( 'NONE',  ( 0.000000000000000000, -0.000000000000000000, 1.000000000000000000 ) ) ;
#1454 = AXIS2_PLACEMENT_3D ( 'NONE', #5080, #4445, #31 ) ;
#1455 = LINE ( 'NONE', #1868, #2834 ) ;
#1456 = VERTEX_POINT ( 'NONE', #4622 ) ;
#1457 = DIRECTION ( 'NONE',  ( -1.820952055660014662E-28, -1.000000000000000000, -7.038118388768679669E-30 ) ) ;
#1458 = DIRECTION ( 'NONE',  ( 0.000000000000000000, 1.000000000000000000, 0.000000000000000000 ) ) ;
#1459 = CARTESIAN_POINT ( 'NONE',  ( 12.20000000000000107, 0.000000000000000000, 0.000000000000000000 ) ) ;
#1460 = CARTESIAN_POINT ( 'NONE',  ( 28.37252191822215863, 30.00000000000000000, -6.000000000000006217 ) ) ;
#1461 = EDGE_CURVE ( 'NONE', #4111, #7715, #7706, .T. ) ;
#1462 = DIRECTION ( 'NONE',  ( 0.000000000000000000, 0.000000000000000000, 1.000000000000000000 ) ) ;
#1463 = CIRCLE ( 'NONE', #6506, 1.899999999999999689 ) ;
#1464 = VECTOR ( 'NONE', #9037, 1000.000000000000000 ) ;
#1465 = CARTESIAN_POINT ( 'NONE',  ( 31.00000000000001066, 27.61361909880193011, -5.005767756411733771 ) ) ;
#1466 = CARTESIAN_POINT ( 'NONE',  ( 0.000000000000000000, 61.99999999999999289, 0.000000000000000000 ) ) ;
#1467 = VERTEX_POINT ( 'NONE', #78 ) ;
#1468 = LINE ( 'NONE', #8296, #5094 ) ;
#1469 = CARTESIAN_POINT ( 'NONE',  ( -28.87459861216645862, 60.99999999999999289, -15.97678174684361707 ) ) ;
#1470 = EDGE_LOOP ( 'NONE', ( #2860, #4315, #52, #1310 ) ) ;
#1471 = EDGE_CURVE ( 'NONE', #9386, #7724, #9718, .T. ) ;
#1472 = ADVANCED_FACE ( 'NONE', ( #4524 ), #7680, .F. ) ;
#1473 = EDGE_CURVE ( 'NONE', #6406, #6663, #8319, .T. ) ;
#1474 = DIRECTION ( 'NONE',  ( 0.000000000000000000, 1.000000000000000000, 0.000000000000000000 ) ) ;
#1475 = CYLINDRICAL_SURFACE ( 'NONE', #8450, 1.500000000000000888 ) ;
#1476 = ORIENTED_EDGE ( 'NONE', *, *, #6421, .T. ) ;
#1477 = CARTESIAN_POINT ( 'NONE',  ( 12.57968859814066853, -1.585441976847065115, 36.91571372862268419 ) ) ;
#1478 = VERTEX_POINT ( 'NONE', #2327 ) ;
#1479 = CARTESIAN_POINT ( 'NONE',  ( -33.06426808735054124, 61.99999999999999289, -5.562309845534586294 ) ) ;
#1480 = VECTOR ( 'NONE', #2008, 1000.000000000000000 ) ;
#1481 = FACE_OUTER_BOUND ( 'NONE', #5832, .T. ) ;
#1482 = CARTESIAN_POINT ( 'NONE',  ( -8.216777476527294510, 58.00000000000029132, -23.61111111111107519 ) ) ;
#1483 = SHAPE_REPRESENTATION ( 'Hardened Alloy Threading Chaser Dies', ( #6314 ), #188 ) ;
#1484 = ORIENTED_EDGE ( 'NONE', *, *, #8532, .F. ) ;
#1485 = FACE_OUTER_BOUND ( 'NONE', #3829, .T. ) ;
#1486 = VERTEX_POINT ( 'NONE', #5357 ) ;
#1487 = EDGE_CURVE ( 'NONE', #2912, #3082, #1601, .T. ) ;
#1488 = DIRECTION ( 'NONE',  ( 0.000000000000000000, 0.000000000000000000, 1.000000000000000000 ) ) ;
#1489 = EDGE_CURVE ( 'NONE', #3682, #6660, #4668, .T. ) ;
#1490 = CARTESIAN_POINT ( 'NONE',  ( -12.43339847825378719, 59.99999999999999289, 35.90836395996003461 ) ) ;
#1491 = DIRECTION ( 'NONE',  ( 0.9449569463147373671, -0.000000000000000000, 0.3271946967961530395 ) ) ;
#1492 = AXIS2_PLACEMENT_3D ( 'NONE', #5946, #9563, #3628 ) ;
#1493 = EDGE_LOOP ( 'NONE', ( #5313, #1972, #8810, #7065, #865, #8191, #3523, #2144 ) ) ;
#1494 = CARTESIAN_POINT ( 'NONE',  ( -6.957283601945606577, 59.12244502749634023, 35.14908888799237729 ) ) ;
#1495 = VERTEX_POINT ( 'NONE', #5593 ) ;
#1496 = UNCERTAINTY_MEASURE_WITH_UNIT (LENGTH_MEASURE( 1.000000000000000082E-05 ), #3676, 'distance_accuracy_value', 'NONE');
#1497 = CIRCLE ( 'NONE', #2113, 26.00000000000008171 ) ;
#1498 = VERTEX_POINT ( 'NONE', #1052 ) ;
#1499 = CARTESIAN_POINT ( 'NONE',  ( -33.06426808735054124, 61.99999999999999289, -5.562309845534586294 ) ) ;
#1500 = AXIS2_PLACEMENT_3D ( 'NONE', #2870, #8858, #6668 ) ;
#1501 =( NAMED_UNIT ( * ) SI_UNIT ( $, .STERADIAN. ) SOLID_ANGLE_UNIT ( ) );
#1502 = DIRECTION ( 'NONE',  ( -0.7071067811865573427, 0.7071067811865376918, 1.533293416683393860E-16 ) ) ;
#1503 = B_SPLINE_CURVE_WITH_KNOTS ( 'NONE', 3,
 ( #7866, #2556, #1142, #2609, #407, #1920 ),
 .UNSPECIFIED., .F., .F.,
 ( 4, 2, 4 ),
 ( 0.000000000000000000, 0.0005212762617847652939, 0.001042552523569530588 ),
 .UNSPECIFIED. ) ;
#1504 = CARTESIAN_POINT ( 'NONE',  ( 2.204364238465235033E-15, 1.000000000000014655, 17.99999999999999645 ) ) ;
#1505 = CARTESIAN_POINT ( 'NONE',  ( -0.02206928620401079830, -9.470079073673241865, 39.52734620791224529 ) ) ;
#1506 = VECTOR ( 'NONE', #1244, 1000.000000000000000 ) ;
#1507 = AXIS2_PLACEMENT_3D ( 'NONE', #6375, #4856, #7920 ) ;
#1508 = AXIS2_PLACEMENT_3D ( 'NONE', #9599, #2269, #6957 ) ;
#1509 = ADVANCED_FACE ( 'NONE', ( #1840 ), #5771, .T. ) ;
#1510 = CARTESIAN_POINT ( 'NONE',  ( -32.99503133754566875, 59.99860354191589806, -3.062309845534580077 ) ) ;
#1511 = ORIENTED_EDGE ( 'NONE', *, *, #1307, .T. ) ;
#1512 = DIRECTION ( 'NONE',  ( 1.735493991486228214E-29, 0.000000000000000000, -1.000000000000000000 ) ) ;
#1513 = LINE ( 'NONE', #827, #8456 ) ;
#1514 = DIRECTION ( 'NONE',  ( 0.000000000000000000, 0.000000000000000000, 1.000000000000000000 ) ) ;
#1515 = EDGE_CURVE ( 'NONE', #4632, #1356, #2598, .T. ) ;
#1516 = AXIS2_PLACEMENT_3D ( 'NONE', #3381, #3570, #9421 ) ;
#1517 = CARTESIAN_POINT ( 'NONE',  ( -1.435128562106514627, -15.00000000000000000, 30.37910620731054934 ) ) ;
#1518 = DIRECTION ( 'NONE',  ( -0.000000000000000000, 1.000000000000000000, -0.000000000000000000 ) ) ;
#1519 = VERTEX_POINT ( 'NONE', #8613 ) ;
#1520 = DIRECTION ( 'NONE',  ( 0.000000000000000000, 0.000000000000000000, -1.000000000000000000 ) ) ;
#1521 = VECTOR ( 'NONE', #4246, 1000.000000000000000 ) ;
#1522 = PLANE ( 'NONE',  #3401 ) ;
#1523 = CARTESIAN_POINT ( 'NONE',  ( 1.820000000000000062, 0.000000000000000000, 0.000000000000000000 ) ) ;
#1524 = ORIENTED_EDGE ( 'NONE', *, *, #7025, .F. ) ;
#1525 = LINE ( 'NONE', #6847, #5872 ) ;
#1526 = CARTESIAN_POINT ( 'NONE',  ( 3.475328499451850295, -15.00000000000000000, 29.62685825611925949 ) ) ;
#1527 = VERTEX_POINT ( 'NONE', #365 ) ;
#1528 = ADVANCED_FACE ( 'NONE', ( #3970 ), #3263, .F. ) ;
#1529 = FACE_OUTER_BOUND ( 'NONE', #5875, .T. ) ;
#1530 = CARTESIAN_POINT ( 'NONE',  ( -6.000000000000005329, 30.00000000000000000, -28.37252191822215863 ) ) ;
#1531 = ORIENTED_EDGE ( 'NONE', *, *, #5980, .F. ) ;
#1532 = CARTESIAN_POINT ( 'NONE',  ( 8.973048768580328627, 7.721000296853482325, 41.89150708015632318 ) ) ;
#1533 = EDGE_CURVE ( 'NONE', #2965, #1437, #1818, .T. ) ;
#1534 = ITEM_DEFINED_TRANSFORMATION ( 'NONE', 'NONE', #4752,  #6314 ) ;
#1535 = ORIENTED_EDGE ( 'NONE', *, *, #7835, .F. ) ;
#1536 = VERTEX_POINT ( 'NONE', #7167 ) ;
#1537 = CARTESIAN_POINT ( 'NONE',  ( -26.32489316217636954, 30.00000000000000000, -5.999999999999995559 ) ) ;
#1538 = EDGE_CURVE ( 'NONE', #928, #8583, #4199, .T. ) ;
#1539 = FACE_OUTER_BOUND ( 'NONE', #941, .T. ) ;
#1540 = CARTESIAN_POINT ( 'NONE',  ( -12.16083066526040213, 60.00000000000029843, -34.94444444444452103 ) ) ;
#1541 = ORIENTED_EDGE ( 'NONE', *, *, #8719, .F. ) ;
#1542 = DIRECTION ( 'NONE',  ( 1.000000000000000000, 0.000000000000000000, 0.000000000000000000 ) ) ;
#1543 = ORIENTED_EDGE ( 'NONE', *, *, #9095, .T. ) ;
#1544 = EDGE_CURVE ( 'NONE', #4065, #6089, #8561, .T. ) ;
#1545 = CARTESIAN_POINT ( 'NONE',  ( -9.476145798193694958, 6.556557297351624847, 41.64275554677251989 ) ) ;
#1546 = DIRECTION ( 'NONE',  ( 0.000000000000000000, 1.000000000000000000, 0.000000000000000000 ) ) ;
#1547 = CARTESIAN_POINT ( 'NONE',  ( -1.350099534931790579, -6.635463807265971070, 43.96408345250505079 ) ) ;
#1548 = EDGE_CURVE ( 'NONE', #7738, #167, #6424, .T. ) ;
#1549 = EDGE_CURVE ( 'NONE', #5397, #3824, #7873, .T. ) ;
#1550 = EDGE_CURVE ( 'NONE', #1104, #4952, #1930, .T. ) ;
#1551 = ORIENTED_EDGE ( 'NONE', *, *, #5337, .F. ) ;
#1552 = CARTESIAN_POINT ( 'NONE',  ( 1.300000000000000044, -0.7216878364870317197, -1.250000000000000000 ) ) ;
#1553 = EDGE_CURVE ( 'NONE', #1933, #9639, #1975, .T. ) ;
#1554 = ORIENTED_EDGE ( 'NONE', *, *, #7273, .T. ) ;
#1555 = ORIENTED_EDGE ( 'NONE', *, *, #5644, .T. ) ;
#1556 = LINE ( 'NONE', #7309, #3942 ) ;
#1557 = CARTESIAN_POINT ( 'NONE',  ( -1.781073977724889623, -11.60243029782703594, 38.96871605616770751 ) ) ;
#1558 = LINE ( 'NONE', #5466, #5093 ) ;
#1559 = ORIENTED_EDGE ( 'NONE', *, *, #2067, .F. ) ;
#1560 = CARTESIAN_POINT ( 'NONE',  ( -32.85680095556730862, 59.99999999999999289, -3.070933240276025877 ) ) ;
#1561 = DIRECTION ( 'NONE',  ( 0.000000000000000000, 0.000000000000000000, -1.000000000000000000 ) ) ;
#1562 = ORIENTED_EDGE ( 'NONE', *, *, #1489, .F. ) ;
#1563 = DIRECTION ( 'NONE',  ( 1.000000000000000000, 0.000000000000000000, 0.000000000000000000 ) ) ;
#1564 = CARTESIAN_POINT ( 'NONE',  ( 0.000000000000000000, 30.00000000000000000, 0.000000000000000000 ) ) ;
#1565 = LINE ( 'NONE', #9024, #4826 ) ;
#1566 = CARTESIAN_POINT ( 'NONE',  ( 33.00000000000000711, 54.99999999999999289, 1.152188841818234638E-13 ) ) ;
#1567 = CIRCLE ( 'NONE', #2813, 1.500000000000001332 ) ;
#1568 = DIRECTION ( 'NONE',  ( 0.000000000000000000, 0.000000000000000000, 1.000000000000000000 ) ) ;
#1569 = SURFACE_STYLE_USAGE ( .BOTH. , #2296 ) ;
#1570 = DIRECTION ( 'NONE',  ( 0.000000000000000000, 0.000000000000000000, 1.000000000000000000 ) ) ;
#1571 = ORIENTED_EDGE ( 'NONE', *, *, #7347, .F. ) ;
#1572 = CARTESIAN_POINT ( 'NONE',  ( 4.000000000000008882, 30.00000000000000000, 29.00000000000000355 ) ) ;
#1573 = AXIS2_PLACEMENT_3D ( 'NONE', #3959, #5445, #2315 ) ;
#1574 = CIRCLE ( 'NONE', #9304, 38.00000000000000000 ) ;
#1575 = DIRECTION ( 'NONE',  ( 1.000000000000000000, 0.000000000000000000, 0.000000000000000000 ) ) ;
#1576 = VECTOR ( 'NONE', #3746, 1000.000000000000114 ) ;
#1577 = PRODUCT_DEFINITION_SHAPE ( 'NONE', 'NONE',  #436 ) ;
#1578 = EDGE_LOOP ( 'NONE', ( #4422, #3915, #177, #9494, #3197 ) ) ;
#1579 = CARTESIAN_POINT ( 'NONE',  ( 0.000000000000000000, 0.000000000000000000, 1.999999999999999556 ) ) ;
#1580 = CARTESIAN_POINT ( 'NONE',  ( 4.481683998297255833, -15.00000000000000000, 29.20001163310385905 ) ) ;
#1581 = ORIENTED_EDGE ( 'NONE', *, *, #7790, .T. ) ;
#1582 = PLANE ( 'NONE',  #1927 ) ;
#1583 = VECTOR ( 'NONE', #8478, 1000.000000000000000 ) ;
#1584 = DIRECTION ( 'NONE',  ( 0.000000000000000000, 0.000000000000000000, 1.000000000000000000 ) ) ;
#1585 = ORIENTED_EDGE ( 'NONE', *, *, #6897, .T. ) ;
#1586 = CARTESIAN_POINT ( 'NONE',  ( 13.12535147532733504, 5.736527869694620918, 36.72510388254905678 ) ) ;
#1587 = CONTEXT_DEPENDENT_SHAPE_REPRESENTATION ( #3791, #1112 ) ;
#1588 = ADVANCED_FACE ( 'NONE', ( #7060 ), #8708, .T. ) ;
#1589 = ORIENTED_EDGE ( 'NONE', *, *, #1841, .F. ) ;
#1590 = FACE_OUTER_BOUND ( 'NONE', #4470, .T. ) ;
#1591 = CARTESIAN_POINT ( 'NONE',  ( -24.67792535850613334, 28.99999999999997158, 4.000000000000009770 ) ) ;
#1592 = PLANE ( 'NONE',  #6541 ) ;
#1593 = DIRECTION ( 'NONE',  ( 0.3286710990611141914, 0.000000000000000000, 0.9444444444444359821 ) ) ;
#1594 = CIRCLE ( 'NONE', #2048, 38.00000000000000711 ) ;
#1595 = VERTEX_POINT ( 'NONE', #5690 ) ;
#1596 = CARTESIAN_POINT ( 'NONE',  ( -2.000890828875744099, 27.95155599451149442, -31.00000000000001066 ) ) ;
#1597 = CARTESIAN_POINT ( 'NONE',  ( 29.00000000000000355, 28.99999999999997158, -4.000000000000007105 ) ) ;
#1598 = CARTESIAN_POINT ( 'NONE',  ( 4.904043666719842598, 61.99999999999999289, 31.11591804390326743 ) ) ;
#1599=STYLED_ITEM('',(#9799),#9696);
#1600 = ORIENTED_EDGE ( 'NONE', *, *, #3220, .F. ) ;
#1601 = LINE ( 'NONE', #6873, #3070 ) ;
#1602 = EDGE_LOOP ( 'NONE', ( #8995, #8351, #1554, #5556 ) ) ;
#1603 = ORIENTED_EDGE ( 'NONE', *, *, #4430, .T. ) ;
#1604 = AXIS2_PLACEMENT_3D ( 'NONE', #7690, #923, #3935 ) ;
#1605 = DIRECTION ( 'NONE',  ( -1.820952055660014662E-28, -1.000000000000000000, 6.508102468073347395E-30 ) ) ;
#1606 = EDGE_CURVE ( 'NONE', #2818, #7534, #9471, .T. ) ;
#1607 = DIRECTION ( 'NONE',  ( -1.000000000000000000, 0.000000000000000000, 0.000000000000000000 ) ) ;
#1608 = ADVANCED_FACE ( 'NONE', ( #2770 ), #8802, .F. ) ;
#1609 = EDGE_CURVE ( 'NONE', #5153, #1498, #3549, .T. ) ;
#1610 = LINE ( 'NONE', #184, #5250 ) ;
#1611 = ORIENTED_EDGE ( 'NONE', *, *, #831, .F. ) ;
#1612 = CARTESIAN_POINT ( 'NONE',  ( 0.000000000000000000, 59.99999999999999289, 38.00000000000000711 ) ) ;
#1613 = EDGE_LOOP ( 'NONE', ( #3161, #8396 ) ) ;
#1614 = CARTESIAN_POINT ( 'NONE',  ( 6.611979057083408939, -4.234811449640147885, 42.87340679459065029 ) ) ;
#1615 = CIRCLE ( 'NONE', #8233, 40.00000000000000711 ) ;
#1616 = CARTESIAN_POINT ( 'NONE',  ( -5.562309845534584518, 49.99999999999999289, 30.56426808735054124 ) ) ;
#1617 = LINE ( 'NONE', #3033, #2215 ) ;
#1618 = PLANE ( 'NONE',  #8218 ) ;
#1619 = DIRECTION ( 'NONE',  ( 0.000000000000000000, 1.000000000000000000, 0.000000000000000000 ) ) ;
#1620 = ORIENTED_EDGE ( 'NONE', *, *, #468, .T. ) ;
#1621 = PLANE ( 'NONE',  #6048 ) ;
#1622 = VECTOR ( 'NONE', #3734, 1000.000000000000000 ) ;
#1623 = DIRECTION ( 'NONE',  ( 0.000000000000000000, 0.000000000000000000, 1.000000000000000000 ) ) ;
#1624 = ORIENTED_EDGE ( 'NONE', *, *, #1897, .T. ) ;
#1625 = DIRECTION ( 'NONE',  ( 0.000000000000000000, 0.000000000000000000, -1.000000000000000000 ) ) ;
#1626 = CARTESIAN_POINT ( 'NONE',  ( 8.821391692846543009, -15.00000000000000178, 36.98463040684644909 ) ) ;
#1627 = AXIS2_PLACEMENT_3D ( 'NONE', #2168, #1491, #8069 ) ;
#1628 = CIRCLE ( 'NONE', #7297, 1.500000000000001332 ) ;
#1629 = ORIENTED_EDGE ( 'NONE', *, *, #5644, .F. ) ;
#1630 = CARTESIAN_POINT ( 'NONE',  ( -15.97678174684350871, 61.99999999999999289, 28.87459861216650836 ) ) ;
#1631 = DIRECTION ( 'NONE',  ( 0.000000000000000000, 0.000000000000000000, 1.000000000000000000 ) ) ;
#1632 = CARTESIAN_POINT ( 'NONE',  ( 8.719889270409380444, -1.642155660953823926, 38.16040262559969420 ) ) ;
#1633 = EDGE_CURVE ( 'NONE', #2537, #7542, #1204, .T. ) ;
#1634 = ORIENTED_EDGE ( 'NONE', *, *, #7005, .F. ) ;
#1635 = LINE ( 'NONE', #7567, #2917 ) ;
#1636 = CARTESIAN_POINT ( 'NONE',  ( 24.96033808169876878, 29.33187429063046991, 4.331874290630486790 ) ) ;
#1637 = VERTEX_POINT ( 'NONE', #2023 ) ;
#1638 = DIRECTION ( 'NONE',  ( 0.000000000000000000, -1.000000000000000000, 0.000000000000000000 ) ) ;
#1639 = VERTEX_POINT ( 'NONE', #7966 ) ;
#1640 = DIRECTION ( 'NONE',  ( -0.000000000000000000, -1.000000000000000000, -0.000000000000000000 ) ) ;
#1641 = CYLINDRICAL_SURFACE ( 'NONE', #1783, 4.500000000000003553 ) ;
#1642 = AXIS2_PLACEMENT_3D ( 'NONE', #3342, #6891, #6351 ) ;
#1643 = ORIENTED_EDGE ( 'NONE', *, *, #1775, .T. ) ;
#1644 = DIRECTION ( 'NONE',  ( 0.000000000000000000, 0.000000000000000000, 1.000000000000000000 ) ) ;
#1645 = ORIENTED_EDGE ( 'NONE', *, *, #821, .F. ) ;
#1646 = ORIENTED_EDGE ( 'NONE', *, *, #6791, .F. ) ;
#1647 = CARTESIAN_POINT ( 'NONE',  ( -1.109536816265070058, -6.661247609618464516, 38.99263510515930165 ) ) ;
#1648 = AXIS2_PLACEMENT_3D ( 'NONE', #6876, #1502, #3121 ) ;
#1649 = CIRCLE ( 'NONE', #7164, 1.999999999999999556 ) ;
#1650 = CARTESIAN_POINT ( 'NONE',  ( 33.06426808735054124, 60.99999999999999289, 8.062309845534588959 ) ) ;
#1651 = PRODUCT_DEFINITION_SHAPE ( 'NONE', 'NONE',  #9763 ) ;
#1652 = VERTEX_POINT ( 'NONE', #1342 ) ;
#1653 = DIRECTION ( 'NONE',  ( -0.000000000000000000, -1.000000000000000000, -0.000000000000000000 ) ) ;
#1654 = CARTESIAN_POINT ( 'NONE',  ( 8.455602827837720289E-27, 41.50000000000020606, -25.00000000000000000 ) ) ;
#1655 = VECTOR ( 'NONE', #8004, 1000.000000000000000 ) ;
#1656 = ADVANCED_FACE ( 'NONE', ( #9542 ), #4222, .F. ) ;
#1657 = AXIS2_PLACEMENT_3D ( 'NONE', #3222, #3024, #3978 ) ;
#1658 = ORIENTED_EDGE ( 'NONE', *, *, #9330, .T. ) ;
#1659 = CARTESIAN_POINT ( 'NONE',  ( 8.955614711045242871, -1.166416508362459137, 41.89990723123212035 ) ) ;
#1660 = ADVANCED_FACE ( 'NONE', ( #8753 ), #2118, .F. ) ;
#1661 = CARTESIAN_POINT ( 'NONE',  ( 31.00000000000000711, 27.42469319230600533, -6.000000000000006217 ) ) ;
#1662 = DIRECTION ( 'NONE',  ( 0.000000000000000000, -0.000000000000000000, -1.000000000000000000 ) ) ;
#1663 = ADVANCED_FACE ( 'NONE', ( #4367 ), #3465, .F. ) ;
#1664 = CARTESIAN_POINT ( 'NONE',  ( -26.32489316217636954, -10.00000000000000533, 6.000000000000009770 ) ) ;
#1665 = VERTEX_POINT ( 'NONE', #1295 ) ;
#1666 = DIRECTION ( 'NONE',  ( -0.1666666666666658525, -3.897465909857536228E-29, -0.9860132971832695770 ) ) ;
#1667 = AXIS2_PLACEMENT_3D ( 'NONE', #559, #6652, #603 ) ;
#1668 = VECTOR ( 'NONE', #4122, 1000.000000000000114 ) ;
#1669 = AXIS2_PLACEMENT_3D ( 'NONE', #7593, #4434, #3685 ) ;
#1670 = VECTOR ( 'NONE', #1457, 1000.000000000000000 ) ;
#1671 = CIRCLE ( 'NONE', #7981, 18.51991245392837371 ) ;
#1672 = EDGE_CURVE ( 'NONE', #7720, #49, #467, .T. ) ;
#1673 = VECTOR ( 'NONE', #4886, 1000.000000000000000 ) ;
#1674 = AXIS2_PLACEMENT_3D ( 'NONE', #4891, #6361, #2501 ) ;
#1675 = LINE ( 'NONE', #1813, #6043 ) ;
#1676 = EDGE_CURVE ( 'NONE', #5781, #7004, #8605, .T. ) ;
#1677 = EDGE_LOOP ( 'NONE', ( #2866, #1524, #8500, #3556 ) ) ;
#1678 = DIRECTION ( 'NONE',  ( 0.000000000000000000, 0.000000000000000000, -1.000000000000000000 ) ) ;
#1679 = LINE ( 'NONE', #2542, #7677 ) ;
#1680 = EDGE_LOOP ( 'NONE', ( #6037, #5607, #3662 ) ) ;
#1681 = LINE ( 'NONE', #6112, #2535 ) ;
#1682 = CIRCLE ( 'NONE', #1213, 33.00000000000000711 ) ;
#1683 = DIRECTION ( 'NONE',  ( -1.820952055660014662E-28, -1.000000000000000000, -7.038118388768679669E-30 ) ) ;
#1684 = ORIENTED_EDGE ( 'NONE', *, *, #4456, .F. ) ;
#1685 = CARTESIAN_POINT ( 'NONE',  ( 3.009843071917527535, -11.32397619240443376, 38.88603724746761969 ) ) ;
#1686 = CONTEXT_DEPENDENT_SHAPE_REPRESENTATION ( #3598, #1651 ) ;
#1687 = CARTESIAN_POINT ( 'NONE',  ( -31.18357922838634266, 54.99999999999999289, -10.79742499427304558 ) ) ;
#1688 = CARTESIAN_POINT ( 'NONE',  ( 10.00000000000001421, 3.294852476641296768, 184.6745183374407020 ) ) ;
#1689 = DIRECTION ( 'NONE',  ( -0.000000000000000000, 1.000000000000000000, -0.000000000000000000 ) ) ;
#1690 = ORIENTED_EDGE ( 'NONE', *, *, #3745, .T. ) ;
#1691 = DIRECTION ( 'NONE',  ( 0.000000000000000000, 0.000000000000000000, 1.000000000000000000 ) ) ;
#1692 = VERTEX_POINT ( 'NONE', #4310 ) ;
#1693 = DIRECTION ( 'NONE',  ( 1.735493991486225972E-29, -6.508102468073347395E-30, -1.000000000000000000 ) ) ;
#1694 = EDGE_CURVE ( 'NONE', #5598, #9259, #9709, .T. ) ;
#1695 = CARTESIAN_POINT ( 'NONE',  ( -5.134502662544168317, 61.85904243767789978, 37.56426808735054124 ) ) ;
#1696 = ORIENTED_EDGE ( 'NONE', *, *, #2990, .F. ) ;
#1697 = DIRECTION ( 'NONE',  ( -0.9449569463147371451, 0.000000000000000000, -0.3271946967961539277 ) ) ;
#1698 = ORIENTED_EDGE ( 'NONE', *, *, #3775, .F. ) ;
#1699 = ORIENTED_EDGE ( 'NONE', *, *, #7492, .T. ) ;
#1700 = DIRECTION ( 'NONE',  ( 0.000000000000000000, 0.000000000000000000, 1.000000000000000000 ) ) ;
#1701 = CARTESIAN_POINT ( 'NONE',  ( -28.34870838944214455, 59.99999999999999289, -9.815840903884556212 ) ) ;
#1702 = LINE ( 'NONE', #7586, #6807 ) ;
#1703 = ORIENTED_EDGE ( 'NONE', *, *, #335, .T. ) ;
#1704 = DIRECTION ( 'NONE',  ( 0.000000000000000000, 1.000000000000000000, 0.000000000000000000 ) ) ;
#1705 = CARTESIAN_POINT ( 'NONE',  ( 5.562309845534932684, 60.99999999999999289, -33.06426808735049150 ) ) ;
#1706 = ORIENTED_EDGE ( 'NONE', *, *, #9014, .T. ) ;
#1707 = EDGE_CURVE ( 'NONE', #1097, #5855, #5606, .T. ) ;
#1708 = PLANE ( 'NONE',  #346 ) ;
#1709 = CARTESIAN_POINT ( 'NONE',  ( 7.548108395552117322, 59.38382381638697893, -34.59619211116746840 ) ) ;
#1710 = CARTESIAN_POINT ( 'NONE',  ( 28.87459861216657231, 60.99999999999999289, 15.97678174684340924 ) ) ;
#1711 = CARTESIAN_POINT ( 'NONE',  ( 28.87459861216657231, 60.99999999999999289, 15.97678174684340924 ) ) ;
#1712 = ORIENTED_EDGE ( 'NONE', *, *, #6925, .T. ) ;
#1713 = CYLINDRICAL_SURFACE ( 'NONE', #9378, 4.500000000000004441 ) ;
#1714 = EDGE_CURVE ( 'NONE', #6660, #7461, #5135, .T. ) ;
#1715 = EDGE_CURVE ( 'NONE', #5638, #8408, #6614, .T. ) ;
#1716 = CARTESIAN_POINT ( 'NONE',  ( 9.860761315262647568E-27, 49.00000000000032685, -25.00000000000000000 ) ) ;
#1717 = DIRECTION ( 'NONE',  ( 1.735493991486225972E-29, -6.508102468073347395E-30, -1.000000000000000000 ) ) ;
#1718 = VERTEX_POINT ( 'NONE', #1537 ) ;
#1719 = DIRECTION ( 'NONE',  ( 0.000000000000000000, 0.000000000000000000, -1.000000000000000000 ) ) ;
#1720 = CARTESIAN_POINT ( 'NONE',  ( 36.80315167070719440, 61.92350945662830952, 8.081333402833552171 ) ) ;
#1721 = ORIENTED_EDGE ( 'NONE', *, *, #7076, .F. ) ;
#1722 = EDGE_CURVE ( 'NONE', #9059, #1935, #5195, .T. ) ;
#1723 = DIRECTION ( 'NONE',  ( 0.000000000000000000, 0.000000000000000000, 1.000000000000000000 ) ) ;
#1724 = EDGE_CURVE ( 'NONE', #6115, #7120, #1635, .T. ) ;
#1725 = EDGE_CURVE ( 'NONE', #9714, #1263, #66, .T. ) ;
#1726 = CARTESIAN_POINT ( 'NONE',  ( 5.562309845534933572, 60.99999999999999289, -37.56426808735049150 ) ) ;
#1727 = ORIENTED_EDGE ( 'NONE', *, *, #8490, .T. ) ;
#1728 = AXIS2_PLACEMENT_3D ( 'NONE', #515, #3511, #6519 ) ;
#1729 = VECTOR ( 'NONE', #3773, 1000.000000000000000 ) ;
#1730 = DIRECTION ( 'NONE',  ( 0.000000000000000000, 1.000000000000000000, 0.000000000000000000 ) ) ;
#1731 = CONTEXT_DEPENDENT_SHAPE_REPRESENTATION ( #1891, #3310 ) ;
#1732 = PLANE ( 'NONE',  #9087 ) ;
#1733 = ORIENTED_EDGE ( 'NONE', *, *, #5337, .T. ) ;
#1734 = DIRECTION ( 'NONE',  ( 0.000000000000000000, 1.000000000000000000, 0.000000000000000000 ) ) ;
#1735 = DIRECTION ( 'NONE',  ( 0.000000000000000000, 1.000000000000000000, 0.000000000000000000 ) ) ;
#1736 = VERTEX_POINT ( 'NONE', #7517 ) ;
#1737 = VECTOR ( 'NONE', #6997, 1000.000000000000000 ) ;
#1738 = DIRECTION ( 'NONE',  ( -1.000000000000000000, -0.000000000000000000, -0.000000000000000000 ) ) ;
#1739 = CARTESIAN_POINT ( 'NONE',  ( -0.6917606027332897645, -6.703808575055850483, 43.99931531168492427 ) ) ;
#1740 = CIRCLE ( 'NONE', #6774, 4.500000000000004441 ) ;
#1741 = ORIENTED_EDGE ( 'NONE', *, *, #1606, .F. ) ;
#1742 = CARTESIAN_POINT ( 'NONE',  ( -34.69710844949434403, 59.33700357310857498, -7.462191142828213053 ) ) ;
#1743 = ORIENTED_EDGE ( 'NONE', *, *, #3291, .T. ) ;
#1744 = CARTESIAN_POINT ( 'NONE',  ( 33.72085295419949347, 59.72647237447257851, 7.995677060003923309 ) ) ;
#1745 = ORIENTED_EDGE ( 'NONE', *, *, #646, .F. ) ;
#1746 = ORIENTED_EDGE ( 'NONE', *, *, #7023, .F. ) ;
#1747 = CARTESIAN_POINT ( 'NONE',  ( -13.29481821656429652, 3.809926294481188691, 36.66398517656647016 ) ) ;
#1748 = DIRECTION ( 'NONE',  ( 0.000000000000000000, 1.000000000000000000, 0.000000000000000000 ) ) ;
#1749 = DIRECTION ( 'NONE',  ( -0.000000000000000000, -1.000000000000000000, -0.000000000000000000 ) ) ;
#1750 = VERTEX_POINT ( 'NONE', #6164 ) ;
#1751 = CARTESIAN_POINT ( 'NONE',  ( -8.429686713947083021, 59.63872771225970837, -24.22291101389071244 ) ) ;
#1752 = VERTEX_POINT ( 'NONE', #3916 ) ;
#1753 = DIRECTION ( 'NONE',  ( 0.3286710990610922090, 6.289316826390952918E-29, 0.9444444444444435316 ) ) ;
#1754 = DIRECTION ( 'NONE',  ( 3.491481338843134539E-15, -0.000000000000000000, -1.000000000000000000 ) ) ;
#1755 = DIRECTION ( 'NONE',  ( 0.000000000000000000, 0.000000000000000000, -1.000000000000000000 ) ) ;
#1756 = CARTESIAN_POINT ( 'NONE',  ( -8.545448575588402207, 41.50000000000020606, -24.55555555555572411 ) ) ;
#1757 = DIRECTION ( 'NONE',  ( -0.9444444444444360931, -0.000000000000000000, 0.3286710990611142469 ) ) ;
#1758 = CIRCLE ( 'NONE', #5240, 1.249999999999999778 ) ;
#1759 = LINE ( 'NONE', #151, #7245 ) ;
#1760 = VERTEX_POINT ( 'NONE', #8201 ) ;
#1761 = CARTESIAN_POINT ( 'NONE',  ( -35.90836395996003461, 39.99999999999999289, -12.43339847825377475 ) ) ;
#1762 = ORIENTED_EDGE ( 'NONE', *, *, #6843, .F. ) ;
#1763 = DIRECTION ( 'NONE',  ( -0.000000000000000000, 1.000000000000000000, -0.000000000000000000 ) ) ;
#1764 = DIRECTION ( 'NONE',  ( -1.000000000000000000, 0.000000000000000000, 0.000000000000000000 ) ) ;
#1765 = ORIENTED_EDGE ( 'NONE', *, *, #280, .F. ) ;
#1766 = CIRCLE ( 'NONE', #7287, 1.500000000000001332 ) ;
#1767 = CARTESIAN_POINT ( 'NONE',  ( 0.000000000000000000, 52.29648987751954792, -38.00000000000000711 ) ) ;
#1768 = CARTESIAN_POINT ( 'NONE',  ( 0.000000000000000000, 0.000000000000000000, -29.00000000000000355 ) ) ;
#1769 = CARTESIAN_POINT ( 'NONE',  ( 5.817259163329850935, -4.845482602429197705, 43.12805808941161700 ) ) ;
#1770 = CONTEXT_DEPENDENT_SHAPE_REPRESENTATION ( #4242, #8361 ) ;
#1771 = VECTOR ( 'NONE', #2872, 1000.000000000000000 ) ;
#1772 = DIRECTION ( 'NONE',  ( 0.000000000000000000, 0.000000000000000000, 1.000000000000000000 ) ) ;
#1773 = VECTOR ( 'NONE', #2596, 1000.000000000000000 ) ;
#1774 = EDGE_CURVE ( 'NONE', #987, #8311, #7660, .T. ) ;
#1775 = EDGE_CURVE ( 'NONE', #4511, #1139, #9103, .T. ) ;
#1776 = VERTEX_POINT ( 'NONE', #5967 ) ;
#1777 = CARTESIAN_POINT ( 'NONE',  ( 8.653435754032105718E-27, 47.50000000000033396, 3.062228611575705006E-28 ) ) ;
#1778 = ORIENTED_EDGE ( 'NONE', *, *, #5924, .T. ) ;
#1779 = CYLINDRICAL_SURFACE ( 'NONE', #9255, 30.00000000000001066 ) ;
#1780 = EDGE_CURVE ( 'NONE', #6156, #6996, #5343, .T. ) ;
#1781 = EDGE_LOOP ( 'NONE', ( #1206, #1555, #8468, #4358 ) ) ;
#1782 = DIRECTION ( 'NONE',  ( 0.000000000000000000, -1.000000000000000000, 0.000000000000000000 ) ) ;
#1783 = AXIS2_PLACEMENT_3D ( 'NONE', #133, #5403, #8363 ) ;
#1784 = CARTESIAN_POINT ( 'NONE',  ( 5.562309845534932684, 60.99999999999999289, -33.06426808735049150 ) ) ;
#1785 = DIRECTION ( 'NONE',  ( -1.000000000000000000, 0.000000000000000000, 0.000000000000000000 ) ) ;
#1786 = ORIENTED_EDGE ( 'NONE', *, *, #5350, .F. ) ;
#1787 = CARTESIAN_POINT ( 'NONE',  ( -35.29563341415538247, 59.05475394944627965, -6.702038549863909012 ) ) ;
#1788 = EDGE_CURVE ( 'NONE', #9115, #9126, #3886, .T. ) ;
#1789 = VERTEX_POINT ( 'NONE', #4657 ) ;
#1790 = DIRECTION ( 'NONE',  ( -0.000000000000000000, -1.000000000000000000, -0.000000000000000000 ) ) ;
#1791 = ORIENTED_EDGE ( 'NONE', *, *, #3717, .F. ) ;
#1792 = EDGE_CURVE ( 'NONE', #8477, #9075, #4610, .T. ) ;
#1793 = CARTESIAN_POINT ( 'NONE',  ( -13.18364556721897429, 5.298907180833983155, 36.70413758096341184 ) ) ;
#1794 = CARTESIAN_POINT ( 'NONE',  ( 8.825381377160069573E-27, 47.00000000000034106, -24.09806918451533875 ) ) ;
#1795 = CYLINDRICAL_SURFACE ( 'NONE', #844, 38.00000000000000711 ) ;
#1796 = CIRCLE ( 'NONE', #9227, 30.00000000000000711 ) ;
#1797 = EDGE_LOOP ( 'NONE', ( #8586, #5702, #530, #3613 ) ) ;
#1798 = CARTESIAN_POINT ( 'NONE',  ( 0.000000000000000000, -15.00000000000000000, 0.000000000000000000 ) ) ;
#1799 = VECTOR ( 'NONE', #1312, 1000.000000000000000 ) ;
#1800 = ORIENTED_EDGE ( 'NONE', *, *, #4335, .T. ) ;
#1801 = CARTESIAN_POINT ( 'NONE',  ( -20.00000000000019185, 19.99999999999990763, 4.999999999999814371 ) ) ;
#1802 = LINE ( 'NONE', #1393, #4679 ) ;
#1803 = CARTESIAN_POINT ( 'NONE',  ( 1.555535097482682654E-26, 78.08723716182652197, -25.00000000000000000 ) ) ;
#1804 = AXIS2_PLACEMENT_3D ( 'NONE', #4884, #3448, #9525 ) ;
#1805 = AXIS2_PLACEMENT_3D ( 'NONE', #1328, #9480, #1283 ) ;
#1806 = CYLINDRICAL_SURFACE ( 'NONE', #6458, 38.00000000000000711 ) ;
#1807 = CARTESIAN_POINT ( 'NONE',  ( 30.00000000000000711, 30.00000000000000000, 0.000000000000000000 ) ) ;
#1808 = EDGE_CURVE ( 'NONE', #8204, #4254, #2929, .T. ) ;
#1809 = VECTOR ( 'NONE', #2463, 1000.000000000000114 ) ;
#1810 = PRESENTATION_LAYER_ASSIGNMENT (  '', '', ( #1026 ) ) ;
#1811 = EDGE_CURVE ( 'NONE', #3433, #4254, #4460, .T. ) ;
#1812 = ORIENTED_EDGE ( 'NONE', *, *, #1538, .F. ) ;
#1813 = CARTESIAN_POINT ( 'NONE',  ( -8.216777476527294510, 53.00000000000031974, -23.61111111111111427 ) ) ;
#1814 = CIRCLE ( 'NONE', #5605, 2.500000000000002220 ) ;
#1815 = ORIENTED_EDGE ( 'NONE', *, *, #3378, .F. ) ;
#1816 = FACE_OUTER_BOUND ( 'NONE', #7478, .T. ) ;
#1817 = DIRECTION ( 'NONE',  ( 6.982962677686269866E-15, -0.000000000000000000, -1.000000000000000000 ) ) ;
#1818 = CIRCLE ( 'NONE', #6856, 30.00000000000001066 ) ;
#1819 = ORIENTED_EDGE ( 'NONE', *, *, #7225, .T. ) ;
#1820 = AXIS2_PLACEMENT_3D ( 'NONE', #6636, #3787, #8929 ) ;
#1821 = CARTESIAN_POINT ( 'NONE',  ( -0.6444271763597331226, 13.27961199780309798, 43.99218798305987121 ) ) ;
#1822 = AXIS2_PLACEMENT_3D ( 'NONE', #1010, #6430, #7830 ) ;
#1823 = DIRECTION ( 'NONE',  ( 2.168404344971006649E-16, -0.000000000000000000, 1.000000000000000000 ) ) ;
#1824 = DIRECTION ( 'NONE',  ( -0.000000000000000000, -1.000000000000000000, -0.000000000000000000 ) ) ;
#1825 = VECTOR ( 'NONE', #4108, 1000.000000000000000 ) ;
#1826 = CARTESIAN_POINT ( 'NONE',  ( -0.01628753085184865904, -6.705134819200520901, 38.99999783451422530 ) ) ;
#1827 = CARTESIAN_POINT ( 'NONE',  ( -8.216777476527274970, 78.08723716182652197, -23.61111111111111427 ) ) ;
#1828 = VERTEX_POINT ( 'NONE', #13 ) ;
#1829 = ORIENTED_EDGE ( 'NONE', *, *, #5990, .T. ) ;
#1830 = CARTESIAN_POINT ( 'NONE',  ( -33.06426808735054124, 49.99999999999999289, -5.562309845534581854 ) ) ;
#1831 = CARTESIAN_POINT ( 'NONE',  ( 2.000890828875750316, 27.95155599451150152, 31.00000000000001421 ) ) ;
#1832 = EDGE_CURVE ( 'NONE', #1139, #1536, #8620, .T. ) ;
#1833 = ORIENTED_EDGE ( 'NONE', *, *, #4920, .T. ) ;
#1834 = CIRCLE ( 'NONE', #1516, 1.249999999999999778 ) ;
#1835 = LINE ( 'NONE', #413, #6334 ) ;
#1836 = CARTESIAN_POINT ( 'NONE',  ( 0.000000000000000000, 19.99999999999982236, 39.00000000000002132 ) ) ;
#1837 = ADVANCED_FACE ( 'NONE', ( #7614 ), #6073, .F. ) ;
#1838 = AXIS2_PLACEMENT_3D ( 'NONE', #254, #7042, #7244 ) ;
#1839 = ORIENTED_EDGE ( 'NONE', *, *, #2828, .F. ) ;
#1840 = FACE_OUTER_BOUND ( 'NONE', #5673, .T. ) ;
#1841 = EDGE_CURVE ( 'NONE', #6883, #9419, #8253, .T. ) ;
#1842 = VERTEX_POINT ( 'NONE', #3711 ) ;
#1843 = FACE_OUTER_BOUND ( 'NONE', #379, .T. ) ;
#1844 = ORIENTED_EDGE ( 'NONE', *, *, #7508, .T. ) ;
#1845 = CARTESIAN_POINT ( 'NONE',  ( -6.066055860285464618, -4.695835677951882836, 38.62830766617436495 ) ) ;
#1846 = CARTESIAN_POINT ( 'NONE',  ( 32.59762842694625817, 61.99999999999999289, -5.137569555611371186 ) ) ;
#1847 = DIRECTION ( 'NONE',  ( 0.000000000000000000, 0.000000000000000000, -1.000000000000000000 ) ) ;
#1848 = EDGE_CURVE ( 'NONE', #7524, #9587, #7667, .T. ) ;
#1849 = ADVANCED_FACE ( 'NONE', ( #1590 ), #3106, .F. ) ;
#1850 = ORIENTED_EDGE ( 'NONE', *, *, #1714, .T. ) ;
#1851 = DIRECTION ( 'NONE',  ( -0.000000000000000000, -1.000000000000000000, -0.000000000000000000 ) ) ;
#1852 = ORIENTED_EDGE ( 'NONE', *, *, #3562, .T. ) ;
#1853 = DIRECTION ( 'NONE',  ( 1.735493991486225972E-29, -6.508102468073347395E-30, -1.000000000000000000 ) ) ;
#1854 = FACE_BOUND ( 'NONE', #8943, .T. ) ;
#1855 = DIRECTION ( 'NONE',  ( 0.000000000000000000, 1.000000000000000000, 0.000000000000000000 ) ) ;
#1856 = DIRECTION ( 'NONE',  ( 0.000000000000000000, 0.000000000000000000, 1.000000000000000000 ) ) ;
#1857 = DIRECTION ( 'NONE',  ( 0.000000000000000000, 0.000000000000000000, 1.000000000000000000 ) ) ;
#1858 = CARTESIAN_POINT ( 'NONE',  ( 8.677469957431129860E-27, 43.00000000000019895, -37.00000000000000711 ) ) ;
#1859 = ORIENTED_EDGE ( 'NONE', *, *, #4933, .F. ) ;
#1860 = CARTESIAN_POINT ( 'NONE',  ( 8.406299021261407051E-27, 42.50000000000020606, -26.00000000000017408 ) ) ;
#1861 = ORIENTED_EDGE ( 'NONE', *, *, #163, .F. ) ;
#1862 = CARTESIAN_POINT ( 'NONE',  ( 8.634329568050956638, 61.97962948615073486, -36.36986309197408218 ) ) ;
#1863 = PRODUCT_DEFINITION ( 'UNKNOWN', '', #2057, #6030 ) ;
#1864 = VERTEX_POINT ( 'NONE', #4507 ) ;
#1865 = CARTESIAN_POINT ( 'NONE',  ( -13.15180771621593792, 5.587517427209601095, 36.71572060651241287 ) ) ;
#1866 = CARTESIAN_POINT ( 'NONE',  ( 36.86535760663189620, 61.99999999999999289, 3.153634179030289530 ) ) ;
#1867 = CARTESIAN_POINT ( 'NONE',  ( 28.33333333333337833, 59.99999999999999289, -9.860132971832594961 ) ) ;
#1868 = CARTESIAN_POINT ( 'NONE',  ( 1.084683744678891232E-26, 53.00000000000031974, -37.00000000000000711 ) ) ;
#1869 = CARTESIAN_POINT ( 'NONE',  ( -30.00000000000001066, 59.99999999999999289, -3.252551416882082410E-13 ) ) ;
#1870 = ORIENTED_EDGE ( 'NONE', *, *, #3165, .F. ) ;
#1871 = DIRECTION ( 'NONE',  ( -1.820952055660014662E-28, -1.000000000000000000, -7.038118388768679669E-30 ) ) ;
#1872 = LINE ( 'NONE', #4008, #1050 ) ;
#1873 = ORIENTED_EDGE ( 'NONE', *, *, #5227, .F. ) ;
#1874 = DIRECTION ( 'NONE',  ( 1.000000000000000000, 0.000000000000000000, 0.000000000000000000 ) ) ;
#1875 = AXIS2_PLACEMENT_3D ( 'NONE', #8965, #621, #2879 ) ;
#1876 = DIRECTION ( 'NONE',  ( -0.000000000000000000, -1.000000000000000000, -0.000000000000000000 ) ) ;
#1877 = EDGE_CURVE ( 'NONE', #6765, #7824, #1110, .T. ) ;
#1878 = DIRECTION ( 'NONE',  ( 0.000000000000000000, 0.000000000000000000, 1.000000000000000000 ) ) ;
#1879 = CARTESIAN_POINT ( 'NONE',  ( 32.59762842694625817, 61.99999999999999289, -5.137569555611371186 ) ) ;
#1880 = ORIENTED_EDGE ( 'NONE', *, *, #9032, .T. ) ;
#1881 = DIRECTION ( 'NONE',  ( 0.000000000000000000, 0.000000000000000000, 1.000000000000000000 ) ) ;
#1882 = ORIENTED_EDGE ( 'NONE', *, *, #9537, .F. ) ;
#1883 = CARTESIAN_POINT ( 'NONE',  ( 0.000000000000000000, 0.000000000000000000, 0.000000000000000000 ) ) ;
#1884 = EDGE_LOOP ( 'NONE', ( #1300, #4459, #9241, #2938 ) ) ;
#1885 = CIRCLE ( 'NONE', #8359, 27.00000000000000355 ) ;
#1886 = AXIS2_PLACEMENT_3D ( 'NONE', #5167, #8171, #9065 ) ;
#1887 = ORIENTED_EDGE ( 'NONE', *, *, #7554, .F. ) ;
#1888 = CARTESIAN_POINT ( 'NONE',  ( -9.211085773935334231, -0.6384518674459094267, 38.05061636510622236 ) ) ;
#1889 = FACE_OUTER_BOUND ( 'NONE', #2046, .T. ) ;
#1890 = CARTESIAN_POINT ( 'NONE',  ( 0.000000000000000000, 59.99999999999999289, 0.000000000000000000 ) ) ;
#1891 =( REPRESENTATION_RELATIONSHIP ('NONE','NONE', #5841, #1483 ) REPRESENTATION_RELATIONSHIP_WITH_TRANSFORMATION ( #9633 )SHAPE_REPRESENTATION_RELATIONSHIP( ) );
#1892 = AXIS2_PLACEMENT_3D ( 'NONE', #5608, #4867, #4132 ) ;
#1893 = ORIENTED_EDGE ( 'NONE', *, *, #1548, .F. ) ;
#1894 = SPHERICAL_SURFACE ( 'NONE', #5678, 4.324969328314201888 ) ;
#1895 = ORIENTED_EDGE ( 'NONE', *, *, #3169, .F. ) ;
#1896 = PLANE ( 'NONE',  #2258 ) ;
#1897 = EDGE_CURVE ( 'NONE', #6355, #7824, #7467, .T. ) ;
#1898 = EDGE_CURVE ( 'NONE', #3824, #1931, #7048, .T. ) ;
#1899 = AXIS2_PLACEMENT_3D ( 'NONE', #2856, #3561, #2064 ) ;
#1900 = DIRECTION ( 'NONE',  ( -0.000000000000000000, -1.000000000000000000, -0.000000000000000000 ) ) ;
#1901 = CARTESIAN_POINT ( 'NONE',  ( 8.239768008128093513, 15.08660039710901657, 38.12250742654718039 ) ) ;
#1902 = EDGE_CURVE ( 'NONE', #6149, #8330, #3407, .T. ) ;
#1903 = DIRECTION ( 'NONE',  ( 0.000000000000000000, -1.000000000000000000, 0.000000000000000000 ) ) ;
#1904 = CIRCLE ( 'NONE', #3160, 26.00000000000009592 ) ;
#1905 = EDGE_CURVE ( 'NONE', #9543, #6002, #429, .T. ) ;
#1906 = CARTESIAN_POINT ( 'NONE',  ( 0.000000000000000000, 39.99999999999999289, -30.00000000000000711 ) ) ;
#1907 = ORIENTED_EDGE ( 'NONE', *, *, #8723, .F. ) ;
#1908 = DIRECTION ( 'NONE',  ( 1.000000000000000000, 0.000000000000000000, 3.491481338843134539E-15 ) ) ;
#1909 = CARTESIAN_POINT ( 'NONE',  ( 0.000000000000000000, 30.99999999999998579, 40.00000000000000711 ) ) ;
#1910 = VERTEX_POINT ( 'NONE', #7864 ) ;
#1911 = DIRECTION ( 'NONE',  ( 0.000000000000000000, 1.000000000000000000, 0.000000000000000000 ) ) ;
#1912 = DIRECTION ( 'NONE',  ( -0.9860132971832693549, -1.788557213313974126E-28, 0.1666666666666657970 ) ) ;
#1913 = ORIENTED_EDGE ( 'NONE', *, *, #3038, .F. ) ;
#1914 = CARTESIAN_POINT ( 'NONE',  ( -12.77877500440332170, 7.486973052590117028, 36.84754185667136994 ) ) ;
#1915 = DIRECTION ( 'NONE',  ( 0.000000000000000000, 0.000000000000000000, 1.000000000000000000 ) ) ;
#1916 = AXIS2_PLACEMENT_3D ( 'NONE', #3446, #4935, #5858 ) ;
#1917 = ORIENTED_EDGE ( 'NONE', *, *, #810, .F. ) ;
#1918 = LINE ( 'NONE', #1187, #7645 ) ;
#1919 = EDGE_LOOP ( 'NONE', ( #6865, #4567, #9685, #12, #6940 ) ) ;
#1920 = CARTESIAN_POINT ( 'NONE',  ( 33.06426808735053413, 59.89212256466219486, 8.062309845534588959 ) ) ;
#1921 = CARTESIAN_POINT ( 'NONE',  ( -8.124805145827266983, -15.00000000000000000, 36.91741529765116780 ) ) ;
#1922 = AXIS2_PLACEMENT_3D ( 'NONE', #2760, #5786, #6801 ) ;
#1923 = VERTEX_POINT ( 'NONE', #8594 ) ;
#1924 = DIRECTION ( 'NONE',  ( 0.000000000000000000, 0.000000000000000000, 1.000000000000000000 ) ) ;
#1925 = CARTESIAN_POINT ( 'NONE',  ( 0.000000000000000000, 37.99999999999996447, 0.000000000000000000 ) ) ;
#1926 = ADVANCED_FACE ( 'NONE', ( #9247 ), #3253, .F. ) ;
#1927 = AXIS2_PLACEMENT_3D ( 'NONE', #7561, #2406, #899 ) ;
#1928 = CARTESIAN_POINT ( 'NONE',  ( 6.697485916193928190, 16.26204223369385460, 38.42259331311452542 ) ) ;
#1929 = ORIENTED_EDGE ( 'NONE', *, *, #1549, .T. ) ;
#1930 = LINE ( 'NONE', #6226, #9242 ) ;
#1931 = VERTEX_POINT ( 'NONE', #990 ) ;
#1932 = DIRECTION ( 'NONE',  ( -0.000000000000000000, -1.000000000000000000, -0.000000000000000000 ) ) ;
#1933 = VERTEX_POINT ( 'NONE', #403 ) ;
#1934 = ADVANCED_FACE ( 'NONE', ( #3408 ), #5495, .F. ) ;
#1935 = VERTEX_POINT ( 'NONE', #5443 ) ;
#1936 = CARTESIAN_POINT ( 'NONE',  ( -8.755997409701210543, -1.617811598344234048, 38.15348978656172818 ) ) ;
#1937 = CIRCLE ( 'NONE', #9206, 37.99999999999999289 ) ;
#1938 = CIRCLE ( 'NONE', #7623, 2.499999999999998668 ) ;
#1939 = CARTESIAN_POINT ( 'NONE',  ( 9.219811829770575476E-27, 40.00000000000014921, -37.00000000000000711 ) ) ;
#1940 = CARTESIAN_POINT ( 'NONE',  ( 1.300000000000000044, 3.252606517456513302E-16, 2.499999999999999556 ) ) ;
#1941 = EDGE_LOOP ( 'NONE', ( #4355, #7203, #6076, #9375 ) ) ;
#1942 = DIRECTION ( 'NONE',  ( 0.000000000000000000, 1.000000000000000000, 0.000000000000000000 ) ) ;
#1943 = EDGE_LOOP ( 'NONE', ( #2612, #3823, #430, #7018, #406 ) ) ;
#1944 = FACE_BOUND ( 'NONE', #6139, .T. ) ;
#1945 = CARTESIAN_POINT ( 'NONE',  ( -29.24912810952613640, 29.14236109046821710, -5.999999999999996447 ) ) ;
#1946 = CARTESIAN_POINT ( 'NONE',  ( 7.754649722547835466, 15.49890469874339871, 38.22487108103376841 ) ) ;
#1947 = EDGE_CURVE ( 'NONE', #5164, #2072, #7908, .T. ) ;
#1948 = DIRECTION ( 'NONE',  ( 0.000000000000000000, 1.000000000000000000, 0.000000000000000000 ) ) ;
#1949 = CARTESIAN_POINT ( 'NONE',  ( 5.137569555611264605, 61.99999999999999289, 32.59762842694627949 ) ) ;
#1950 = EDGE_CURVE ( 'NONE', #9118, #8659, #2607, .T. ) ;
#1951 = EDGE_CURVE ( 'NONE', #3761, #8698, #3078, .T. ) ;
#1952 = CIRCLE ( 'NONE', #84, 4.324969328314201888 ) ;
#1953 = ORIENTED_EDGE ( 'NONE', *, *, #8512, .F. ) ;
#1954 = EDGE_CURVE ( 'NONE', #7681, #7154, #8463, .T. ) ;
#1955 = AXIS2_PLACEMENT_3D ( 'NONE', #6201, #251, #200 ) ;
#1956 = DIRECTION ( 'NONE',  ( 0.7849198975831892522, 0.000000000000000000, -0.6195972517514870548 ) ) ;
#1957 = CYLINDRICAL_SURFACE ( 'NONE', #5118, 2.500000000000002220 ) ;
#1958 = ORIENTED_EDGE ( 'NONE', *, *, #9216, .T. ) ;
#1959 = PLANE ( 'NONE',  #3651 ) ;
#1960 = CARTESIAN_POINT ( 'NONE',  ( -4.000000000000005329, 0.000000000000000000, -24.67792535850613334 ) ) ;
#1961 = CARTESIAN_POINT ( 'NONE',  ( 4.898587196589413815E-15, 0.000000000000000000, 40.00000000000000711 ) ) ;
#1962 = PLANE ( 'NONE',  #1454 ) ;
#1963 = AXIS2_PLACEMENT_3D ( 'NONE', #3744, #3794, #1462 ) ;
#1964 = EDGE_CURVE ( 'NONE', #7838, #4449, #4159, .T. ) ;
#1965 = ADVANCED_FACE ( 'NONE', ( #8503 ), #1732, .T. ) ;
#1966 = FACE_OUTER_BOUND ( 'NONE', #6966, .T. ) ;
#1967 = VECTOR ( 'NONE', #9594, 1000.000000000000000 ) ;
#1968 = VECTOR ( 'NONE', #9277, 1000.000000000000000 ) ;
#1969 = VERTEX_POINT ( 'NONE', #5536 ) ;
#1970 = CARTESIAN_POINT ( 'NONE',  ( 16.70299909897254409, 61.99999999999999289, -30.18708036726510002 ) ) ;
#1971 = CARTESIAN_POINT ( 'NONE',  ( -8.643728504328578310, -6.580413251913810768, 38.16276976896127593 ) ) ;
#1972 = ORIENTED_EDGE ( 'NONE', *, *, #7129, .F. ) ;
#1973 = CARTESIAN_POINT ( 'NONE',  ( 13.53485947486097984, 3.294852476641298544, 295.0000000000000000 ) ) ;
#1974 = AXIS2_PLACEMENT_3D ( 'NONE', #5146, #1335, #9536 ) ;
#1975 = CIRCLE ( 'NONE', #5304, 26.00000000000000355 ) ;
#1976 = DIRECTION ( 'NONE',  ( 0.000000000000000000, 0.000000000000000000, 1.000000000000000000 ) ) ;
#1977 = CIRCLE ( 'NONE', #8134, 26.00000000000000355 ) ;
#1978 = EDGE_CURVE ( 'NONE', #3873, #5638, #6998, .T. ) ;
#1979 = CARTESIAN_POINT ( 'NONE',  ( 7.068581912135081247, 16.00861037931602127, 38.35581056696806712 ) ) ;
#1980 = VERTEX_POINT ( 'NONE', #1869 ) ;
#1981 = CARTESIAN_POINT ( 'NONE',  ( -33.89029069002005912, 59.89318186371823316, -3.196943324609351045 ) ) ;
#1982 = AXIS2_PLACEMENT_3D ( 'NONE', #7594, #3936, #7785 ) ;
#1983 = EDGE_LOOP ( 'NONE', ( #9554, #3770, #3275, #7476, #80 ) ) ;
#1984 = CARTESIAN_POINT ( 'NONE',  ( 35.47893788052810038, 58.98370868798952671, 6.231324730575376059 ) ) ;
#1985 = EDGE_LOOP ( 'NONE', ( #6670, #9493, #5390, #2665, #2718 ) ) ;
#1986 = ORIENTED_EDGE ( 'NONE', *, *, #3474, .F. ) ;
#1987 = CARTESIAN_POINT ( 'NONE',  ( -8.768074816142425121, 14.61274975128556264, 38.00682554133690871 ) ) ;
#1988 = EDGE_CURVE ( 'NONE', #6362, #8659, #4361, .T. ) ;
#1989 = LINE ( 'NONE', #323, #8924 ) ;
#1990 = DIRECTION ( 'NONE',  ( -0.000000000000000000, -1.000000000000000000, -0.000000000000000000 ) ) ;
#1991 = VECTOR ( 'NONE', #8240, 1000.000000000000000 ) ;
#1992 = VERTEX_POINT ( 'NONE', #7712 ) ;
#1993 = LINE ( 'NONE', #2083, #4983 ) ;
#1994 = ORIENTED_EDGE ( 'NONE', *, *, #7366, .F. ) ;
#1995 = CARTESIAN_POINT ( 'NONE',  ( -15.97678174684350871, 60.99999999999999289, 28.87459861216650836 ) ) ;
#1996 = CARTESIAN_POINT ( 'NONE',  ( 8.948640893600852668E-27, 42.50000000000020606, -24.09806918451538849 ) ) ;
#1997 = DIRECTION ( 'NONE',  ( 0.000000000000000000, -0.000000000000000000, 1.000000000000000000 ) ) ;
#1998 = DIRECTION ( 'NONE',  ( 0.000000000000000000, 1.000000000000000000, 0.000000000000000000 ) ) ;
#1999 = CARTESIAN_POINT ( 'NONE',  ( -33.06426808735054124, 69.99999999999998579, -5.562309845534581854 ) ) ;
#2000 = ADVANCED_FACE ( 'NONE', ( #6264 ), #8547, .T. ) ;
#2001 = VERTEX_POINT ( 'NONE', #3956 ) ;
#2002 = CARTESIAN_POINT ( 'NONE',  ( -33.06426808735053413, 59.89212256466219486, -8.062309845534585406 ) ) ;
#2003 = CARTESIAN_POINT ( 'NONE',  ( 5.048957243282207408, 11.93285829901166295, 43.34552440119345107 ) ) ;
#2004 = ORIENTED_EDGE ( 'NONE', *, *, #8668, .F. ) ;
#2005 = DIRECTION ( 'NONE',  ( 7.666467083416968066E-17, -0.7071067811865378028, 0.7071067811865572317 ) ) ;
#2006 = CARTESIAN_POINT ( 'NONE',  ( 35.90836395996004171, 59.99999999999999289, 12.43339847825378186 ) ) ;
#2007 = ADVANCED_FACE ( 'NONE', ( #7804 ), #3303, .T. ) ;
#2008 = DIRECTION ( 'NONE',  ( -0.000000000000000000, -1.000000000000000000, -0.000000000000000000 ) ) ;
#2009 = LINE ( 'NONE', #2979, #2871 ) ;
#2010 = CYLINDRICAL_SURFACE ( 'NONE', #8911, 27.00000000000000355 ) ;
#2011 = ORIENTED_EDGE ( 'NONE', *, *, #760, .T. ) ;
#2012 = CARTESIAN_POINT ( 'NONE',  ( 4.000000000000002665, 0.000000000000000000, -8.673617379884032514E-16 ) ) ;
#2013 = CARTESIAN_POINT ( 'NONE',  ( -11.07761026121418091, -4.999999999999992006, 37.39366993089505797 ) ) ;
#2014 = ORIENTED_EDGE ( 'NONE', *, *, #5120, .T. ) ;
#2015 = EDGE_CURVE ( 'NONE', #2652, #7114, #6681, .T. ) ;
#2016 = ADVANCED_FACE ( 'NONE', ( #9583 ), #2010, .F. ) ;
#2017 = EDGE_CURVE ( 'NONE', #4254, #1750, #5591, .T. ) ;
#2018 = DIRECTION ( 'NONE',  ( 0.000000000000000000, 1.000000000000000000, 0.000000000000000000 ) ) ;
#2019 = DIRECTION ( 'NONE',  ( 0.000000000000000000, 0.000000000000000000, 1.000000000000000000 ) ) ;
#2020 = CARTESIAN_POINT ( 'NONE',  ( 0.5600451362621369222, 13.28348936595889107, 38.99807195037084995 ) ) ;
#2021 = DIRECTION ( 'NONE',  ( -1.000000000000000000, -5.551115123129975991E-17, 1.180727526274980869E-14 ) ) ;
#2022 = ORIENTED_EDGE ( 'NONE', *, *, #280, .T. ) ;
#2023 = CARTESIAN_POINT ( 'NONE',  ( 8.455602827837720289E-27, 41.50000000000020606, -25.00000000000000000 ) ) ;
#2024 = EDGE_LOOP ( 'NONE', ( #205, #7432, #6216, #6428, #3410 ) ) ;
#2025 = DIRECTION ( 'NONE',  ( -1.735493991486225972E-29, 6.508102468073347395E-30, 1.000000000000000000 ) ) ;
#2026 = ORIENTED_EDGE ( 'NONE', *, *, #2441, .F. ) ;
#2027 = CARTESIAN_POINT ( 'NONE',  ( 0.000000000000000000, 0.000000000000000000, 0.000000000000000000 ) ) ;
#2028 = ORIENTED_EDGE ( 'NONE', *, *, #5393, .T. ) ;
#2029 = CARTESIAN_POINT ( 'NONE',  ( -8.216777476527274970, 78.08723716182652197, -23.61111111111111427 ) ) ;
#2030 = DIRECTION ( 'NONE',  ( -0.000000000000000000, -1.000000000000000000, -0.000000000000000000 ) ) ;
#2031 = LINE ( 'NONE', #3670, #7621 ) ;
#2032 = CIRCLE ( 'NONE', #7573, 1.500000000000000888 ) ;
#2033 = AXIS2_PLACEMENT_3D ( 'NONE', #1803, #9225, #9178 ) ;
#2034 = ORIENTED_EDGE ( 'NONE', *, *, #8682, .F. ) ;
#2035 = DIRECTION ( 'NONE',  ( -1.000000000000000000, 0.000000000000000000, -3.083952846180987322E-15 ) ) ;
#2036 = CARTESIAN_POINT ( 'NONE',  ( 1.300000000000000044, 1.443375672974065216, 1.084202172492522584E-16 ) ) ;
#2037 = EDGE_LOOP ( 'NONE', ( #8017, #5431, #7356, #1261 ) ) ;
#2038 = CYLINDRICAL_SURFACE ( 'NONE', #2725, 30.00000000000000711 ) ;
#2039 = CYLINDRICAL_SURFACE ( 'NONE', #8669, 39.00000000000002132 ) ;
#2040 = DIRECTION ( 'NONE',  ( 0.000000000000000000, -1.000000000000000000, 0.000000000000000000 ) ) ;
#2041 = FACE_OUTER_BOUND ( 'NONE', #2679, .T. ) ;
#2042 = DIRECTION ( 'NONE',  ( -0.000000000000000000, -1.000000000000000000, -0.000000000000000000 ) ) ;
#2043 = AXIS2_PLACEMENT_3D ( 'NONE', #4080, #6337, #9358 ) ;
#2044 = DIRECTION ( 'NONE',  ( 0.000000000000000000, 0.000000000000000000, -1.000000000000000000 ) ) ;
#2045 = DIRECTION ( 'NONE',  ( -0.1666666666666658525, -3.897465909857536228E-29, -0.9860132971832695770 ) ) ;
#2046 = EDGE_LOOP ( 'NONE', ( #4339, #1311, #9651, #3812, #6005 ) ) ;
#2047 = DIRECTION ( 'NONE',  ( -0.000000000000000000, 0.000000000000000000, -1.000000000000000000 ) ) ;
#2048 = AXIS2_PLACEMENT_3D ( 'NONE', #8635, #4923, #1857 ) ;
#2049 = PLANE ( 'NONE',  #6677 ) ;
#2050 = ORIENTED_EDGE ( 'NONE', *, *, #3287, .T. ) ;
#2051 = DIRECTION ( 'NONE',  ( -1.820952055660014662E-28, -1.000000000000000000, -7.038118388768679669E-30 ) ) ;
#2052 = DIRECTION ( 'NONE',  ( 0.3286710990611141914, 0.000000000000000000, 0.9444444444444359821 ) ) ;
#2053 = CARTESIAN_POINT ( 'NONE',  ( 30.00000000000000711, 39.99999999999999289, 1.047444401652940259E-13 ) ) ;
#2054 = LINE ( 'NONE', #5774, #6969 ) ;
#2055 = FACE_BOUND ( 'NONE', #7598, .T. ) ;
#2056 = CARTESIAN_POINT ( 'NONE',  ( 9.815840903884561541, 59.99999999999999289, -28.34870838944214100 ) ) ;
#2057 = PRODUCT_DEFINITION_FORMATION_WITH_SPECIFIED_SOURCE ( 'ANY', '', #6053, .NOT_KNOWN. ) ;
#2058 = ORIENTED_EDGE ( 'NONE', *, *, #1461, .F. ) ;
#2059 = CARTESIAN_POINT ( 'NONE',  ( 1.094544505994153880E-26, 52.00000000000031974, -37.00000000000000711 ) ) ;
#2060 = CARTESIAN_POINT ( 'NONE',  ( -8.237197373723452287, -14.99999999999999822, 27.80554943579402405 ) ) ;
#2061 = ORIENTED_EDGE ( 'NONE', *, *, #5948, .F. ) ;
#2062 = CARTESIAN_POINT ( 'NONE',  ( 0.000000000000000000, 59.99999999999999289, 0.000000000000000000 ) ) ;
#2063 = DIRECTION ( 'NONE',  ( 0.000000000000000000, 0.000000000000000000, 1.000000000000000000 ) ) ;
#2064 = DIRECTION ( 'NONE',  ( 0.000000000000000000, 0.000000000000000000, 1.000000000000000000 ) ) ;
#2065 = ORIENTED_EDGE ( 'NONE', *, *, #7997, .T. ) ;
#2066 = CARTESIAN_POINT ( 'NONE',  ( 6.124541788014690624, 11.22654513750760330, 43.03812152903055477 ) ) ;
#2067 = EDGE_CURVE ( 'NONE', #6704, #1432, #9068, .T. ) ;
#2068 = VECTOR ( 'NONE', #997, 1000.000000000000000 ) ;
#2069 = ORIENTED_EDGE ( 'NONE', *, *, #6780, .F. ) ;
#2070 = CARTESIAN_POINT ( 'NONE',  ( 8.012675919994043991E-27, 44.00000000000019895, 2.908154216024726138E-28 ) ) ;
#2071 = ADVANCED_FACE ( 'NONE', ( #8094 ), #9621, .T. ) ;
#2072 = VERTEX_POINT ( 'NONE', #639 ) ;
#2073 = DIRECTION ( 'NONE',  ( 1.735493991486223169E-29, 0.000000000000000000, -1.000000000000000000 ) ) ;
#2074 = ORIENTED_EDGE ( 'NONE', *, *, #586, .F. ) ;
#2075 = CARTESIAN_POINT ( 'NONE',  ( -5.562309845534584518, 49.99999999999999289, 33.06426808735054124 ) ) ;
#2076 = ORIENTED_EDGE ( 'NONE', *, *, #8696, .F. ) ;
#2077 = CARTESIAN_POINT ( 'NONE',  ( -8.102752655081463473, 15.22736282390319040, 38.15602848768372723 ) ) ;
#2078 = CARTESIAN_POINT ( 'NONE',  ( -8.216777476527274970, 49.00000000000032685, -23.61111111111111427 ) ) ;
#2079 = AXIS2_PLACEMENT_3D ( 'NONE', #6062, #3853, #6160 ) ;
#2080 = DIRECTION ( 'NONE',  ( 0.000000000000000000, 0.000000000000000000, 1.000000000000000000 ) ) ;
#2081 = EDGE_CURVE ( 'NONE', #4551, #7854, #399, .T. ) ;
#2082 = ORIENTED_EDGE ( 'NONE', *, *, #290, .T. ) ;
#2083 = CARTESIAN_POINT ( 'NONE',  ( 29.82695610816121956, 59.99999999999999289, -23.54469556655648077 ) ) ;
#2084 = EDGE_CURVE ( 'NONE', #9419, #6457, #5819, .T. ) ;
#2085 = ORIENTED_EDGE ( 'NONE', *, *, #1360, .T. ) ;
#2086 = CARTESIAN_POINT ( 'NONE',  ( 6.000000000000001776, 30.00000000000000000, -31.00000000000000711 ) ) ;
#2087 = AXIS2_PLACEMENT_3D ( 'NONE', #8037, #1277, #450 ) ;
#2088 = CARTESIAN_POINT ( 'NONE',  ( 0.000000000000000000, 3.294852476641296768, 300.0000000000000000 ) ) ;
#2089 = DIRECTION ( 'NONE',  ( 0.000000000000000000, 1.000000000000000000, 0.000000000000000000 ) ) ;
#2090 = CARTESIAN_POINT ( 'NONE',  ( -23.54469556655647722, 59.99999999999999289, -29.82695610816121956 ) ) ;
#2091 = CARTESIAN_POINT ( 'NONE',  ( -5.999999999999998224, -10.00000000000000533, 31.00000000000000711 ) ) ;
#2092 = ORIENTED_EDGE ( 'NONE', *, *, #5656, .T. ) ;
#2093 = DIRECTION ( 'NONE',  ( 0.000000000000000000, 0.000000000000000000, 1.000000000000000000 ) ) ;
#2094 = CARTESIAN_POINT ( 'NONE',  ( 28.34870838944214100, 39.99999999999999289, 9.815840903884559765 ) ) ;
#2095 = CARTESIAN_POINT ( 'NONE',  ( 1.300000000000000044, -1.443375672974064328, -9.326206579303807412E-18 ) ) ;
#2096 = DIRECTION ( 'NONE',  ( -1.820952055660014662E-28, -1.000000000000000000, -7.038118388768679669E-30 ) ) ;
#2097 = DIRECTION ( 'NONE',  ( 0.000000000000000000, 0.000000000000000000, 1.000000000000000000 ) ) ;
#2098 = CARTESIAN_POINT ( 'NONE',  ( 6.439978105601112524E-15, 18.29485247664131009, 39.00000000000002132 ) ) ;
#2099 = ADVANCED_FACE ( 'NONE', ( #5862 ), #8591, .T. ) ;
#2100 = CIRCLE ( 'NONE', #2743, 17.99999999999999645 ) ;
#2101 = DIRECTION ( 'NONE',  ( -0.9449569463147374782, 0.000000000000000000, -0.3271946967961530950 ) ) ;
#2102 = ORIENTED_EDGE ( 'NONE', *, *, #690, .T. ) ;
#2103 = DIRECTION ( 'NONE',  ( 0.000000000000000000, 0.000000000000000000, -1.000000000000000000 ) ) ;
#2104 = CARTESIAN_POINT ( 'NONE',  ( -2.470322857848779918, -15.00000000000000000, 30.03203418347360909 ) ) ;
#2105 = EDGE_LOOP ( 'NONE', ( #4709, #5925, #3468, #1218 ) ) ;
#2106 = CIRCLE ( 'NONE', #870, 33.00000000000000711 ) ;
#2107 = AXIS2_PLACEMENT_3D ( 'NONE', #2753, #597, #2800 ) ;
#2108 = CARTESIAN_POINT ( 'NONE',  ( 4.000000000000001776, 28.99999999999997158, -24.67792535850613334 ) ) ;
#2109 = CARTESIAN_POINT ( 'NONE',  ( 8.677469957431129860E-27, 46.00000000000018474, -26.00000000000012790 ) ) ;
#2110 = CARTESIAN_POINT ( 'NONE',  ( 33.06426808735054124, 59.99999999999999289, 3.062309845534584074 ) ) ;
#2111 = EDGE_LOOP ( 'NONE', ( #5621, #2642, #1441, #9501, #1133, #2058, #8657 ) ) ;
#2112 = CARTESIAN_POINT ( 'NONE',  ( 5.928038920598607042, 16.73037627209208367, 38.54880476822177116 ) ) ;
#2113 = AXIS2_PLACEMENT_3D ( 'NONE', #4462, #8851, #2073 ) ;
#2114 = DIRECTION ( 'NONE',  ( 0.000000000000000000, -1.000000000000000000, 0.000000000000000000 ) ) ;
#2115 = VECTOR ( 'NONE', #1072, 1000.000000000000000 ) ;
#2116 = EDGE_CURVE ( 'NONE', #9587, #6156, #2701, .T. ) ;
#2117 = VERTEX_POINT ( 'NONE', #4352 ) ;
#2118 = CYLINDRICAL_SURFACE ( 'NONE', #7340, 30.00000000000000711 ) ;
#2119 = ORIENTED_EDGE ( 'NONE', *, *, #1000, .T. ) ;
#2120 = CARTESIAN_POINT ( 'NONE',  ( 9.860132971832495485, 59.99999999999999289, 28.33333333333341031 ) ) ;
#2121 = ORIENTED_EDGE ( 'NONE', *, *, #6525, .F. ) ;
#2122 = DIRECTION ( 'NONE',  ( 0.000000000000000000, 1.000000000000000000, 0.000000000000000000 ) ) ;
#2123 = EDGE_LOOP ( 'NONE', ( #8637, #6822, #6319, #1242, #7196 ) ) ;
#2124 = AXIS2_PLACEMENT_3D ( 'NONE', #8654, #2709, #8559 ) ;
#2125 = CARTESIAN_POINT ( 'NONE',  ( -6.594791314557400419, 10.84011732630675695, 42.87949548222016460 ) ) ;
#2126 = VECTOR ( 'NONE', #3661, 1000.000000000000000 ) ;
#2127 = AXIS2_PLACEMENT_3D ( 'NONE', #317, #5507, #8514 ) ;
#2128 = DIRECTION ( 'NONE',  ( 0.000000000000000000, 0.000000000000000000, -1.000000000000000000 ) ) ;
#2129 = TOROIDAL_SURFACE ( 'NONE', #105, 33.00000000000000711, 5.000000000000000000 ) ;
#2130 = EDGE_CURVE ( 'NONE', #3412, #3666, #7250, .T. ) ;
#2131 = CARTESIAN_POINT ( 'NONE',  ( 0.000000000000000000, 37.99999999999996447, 0.000000000000000000 ) ) ;
#2132 = CIRCLE ( 'NONE', #1982, 1.249999999999999778 ) ;
#2133 = VECTOR ( 'NONE', #6212, 1000.000000000000000 ) ;
#2134 = ORIENTED_EDGE ( 'NONE', *, *, #7025, .T. ) ;
#2135 = DIRECTION ( 'NONE',  ( 0.000000000000000000, -1.000000000000000000, 0.000000000000000000 ) ) ;
#2136 = ORIENTED_EDGE ( 'NONE', *, *, #9140, .F. ) ;
#2137 = DIRECTION ( 'NONE',  ( 0.000000000000000000, 0.000000000000000000, 1.000000000000000000 ) ) ;
#2138 = DIRECTION ( 'NONE',  ( 0.000000000000000000, 0.000000000000000000, 1.000000000000000000 ) ) ;
#2139 = EDGE_CURVE ( 'NONE', #4095, #8510, #6049, .T. ) ;
#2140 = SURFACE_STYLE_FILL_AREA ( #5895 ) ;
#2141 = VECTOR ( 'NONE', #299, 1000.000000000000000 ) ;
#2142 = ADVANCED_FACE ( 'NONE', ( #9527 ), #5780, .F. ) ;
#2143 = DIRECTION ( 'NONE',  ( 0.000000000000000000, 0.000000000000000000, 1.000000000000000000 ) ) ;
#2144 = ORIENTED_EDGE ( 'NONE', *, *, #9146, .F. ) ;
#2145 = CARTESIAN_POINT ( 'NONE',  ( -5.562309845534701758, 61.83753588906734677, 37.56426808735052703 ) ) ;
#2146 = CARTESIAN_POINT ( 'NONE',  ( -32.05305536707737701, 59.99999999999999289, -7.848671329280701769 ) ) ;
#2147 = FACE_OUTER_BOUND ( 'NONE', #8893, .T. ) ;
#2148 = PLANE ( 'NONE',  #7284 ) ;
#2149 = DIRECTION ( 'NONE',  ( 0.000000000000000000, 0.000000000000000000, -1.000000000000000000 ) ) ;
#2150 = FACE_OUTER_BOUND ( 'NONE', #3206, .T. ) ;
#2151 = DIRECTION ( 'NONE',  ( 0.000000000000000000, -0.000000000000000000, 1.000000000000000000 ) ) ;
#2152 = VERTEX_POINT ( 'NONE', #7953 ) ;
#2153 = CARTESIAN_POINT ( 'NONE',  ( 0.000000000000000000, 61.99999999999999289, -37.00000000000000711 ) ) ;
#2154 = CARTESIAN_POINT ( 'NONE',  ( 0.4198266780023428568, -14.99999999999984190, 36.76416815479328903 ) ) ;
#2155 = ORIENTED_EDGE ( 'NONE', *, *, #6224, .F. ) ;
#2156 = DIRECTION ( 'NONE',  ( -1.224646799147353207E-16, 1.000000000000000000, 0.000000000000000000 ) ) ;
#2157 = LINE ( 'NONE', #2954, #6691 ) ;
#2158 = CARTESIAN_POINT ( 'NONE',  ( 9.981004741123138402, 4.018542934133168210, 37.86365196549936485 ) ) ;
#2159 = ORIENTED_EDGE ( 'NONE', *, *, #8489, .T. ) ;
#2160 = DIRECTION ( 'NONE',  ( 1.000000000000000000, 0.000000000000000000, -0.000000000000000000 ) ) ;
#2161 = ORIENTED_EDGE ( 'NONE', *, *, #2427, .T. ) ;
#2162 = DIRECTION ( 'NONE',  ( 0.000000000000000000, 1.000000000000000000, 0.000000000000000000 ) ) ;
#2163 = EDGE_LOOP ( 'NONE', ( #1551, #7027, #1812 ) ) ;
#2164 = PLANE ( 'NONE',  #1355 ) ;
#2165 = ORIENTED_EDGE ( 'NONE', *, *, #7583, .T. ) ;
#2166 = CARTESIAN_POINT ( 'NONE',  ( -8.731905042198331302, 8.252142515900809272, 38.15876855944379287 ) ) ;
#2167 = PLANE ( 'NONE',  #3723 ) ;
#2168 = CARTESIAN_POINT ( 'NONE',  ( 10.79742499427305269, 54.99999999999999289, -31.18357922838633911 ) ) ;
#2169 = VERTEX_POINT ( 'NONE', #1236 ) ;
#2170 = CARTESIAN_POINT ( 'NONE',  ( -0.01963426291156584666, -6.705128248126137613, 43.99999014335539016 ) ) ;
#2171 = ADVANCED_FACE ( 'NONE', ( #5679 ), #5136, .T. ) ;
#2172 = ORIENTED_EDGE ( 'NONE', *, *, #3907, .F. ) ;
#2173 = DIRECTION ( 'NONE',  ( 0.000000000000000000, 1.000000000000000000, 0.000000000000000000 ) ) ;
#2174 =( NAMED_UNIT ( * ) SI_UNIT ( $, .STERADIAN. ) SOLID_ANGLE_UNIT ( ) );
#2175 = PLANE ( 'NONE',  #7256 ) ;
#2176 =( LENGTH_UNIT ( ) NAMED_UNIT ( * ) SI_UNIT ( .MILLI., .METRE. ) );
#2177 = CIRCLE ( 'NONE', #7722, 26.00000000000003197 ) ;
#2178 = DIRECTION ( 'NONE',  ( 0.9860132971832693549, 1.788557213313974126E-28, -0.1666666666666657970 ) ) ;
#2179 = ADVANCED_FACE ( 'NONE', ( #1966 ), #8792, .F. ) ;
#2180 = EDGE_CURVE ( 'NONE', #1980, #5194, #8044, .T. ) ;
#2181 = ORIENTED_EDGE ( 'NONE', *, *, #7636, .F. ) ;
#2182 = CARTESIAN_POINT ( 'NONE',  ( 0.6536441304786463347, -6.706450183173051194, 44.00066613171647845 ) ) ;
#2183 = LINE ( 'NONE', #4392, #6528 ) ;
#2184 = EDGE_CURVE ( 'NONE', #6883, #6218, #1918, .T. ) ;
#2185 = CARTESIAN_POINT ( 'NONE',  ( 12.20000000000000107, 0.000000000000000000, 0.000000000000000000 ) ) ;
#2186 = CARTESIAN_POINT ( 'NONE',  ( 4.007921376381021084, 27.80323177039520033, -31.00000000000000711 ) ) ;
#2187 = AXIS2_PLACEMENT_3D ( 'NONE', #9333, #8222, #401 ) ;
#2188 = LINE ( 'NONE', #6792, #4017 ) ;
#2189 = CARTESIAN_POINT ( 'NONE',  ( 31.00000000000000355, 27.99909559099847911, 2.017392264862529760 ) ) ;
#2190 = DIRECTION ( 'NONE',  ( 1.735493991486225411E-29, 0.000000000000000000, -1.000000000000000000 ) ) ;
#2191 = EDGE_CURVE ( 'NONE', #2351, #5863, #6842, .T. ) ;
#2192 = VERTEX_POINT ( 'NONE', #5382 ) ;
#2193 = FACE_OUTER_BOUND ( 'NONE', #5768, .T. ) ;
#2194 = LINE ( 'NONE', #5232, #1991 ) ;
#2195 = ORIENTED_EDGE ( 'NONE', *, *, #223, .F. ) ;
#2196 =( GEOMETRIC_REPRESENTATION_CONTEXT ( 3 ) GLOBAL_UNCERTAINTY_ASSIGNED_CONTEXT ( ( #3771 ) ) GLOBAL_UNIT_ASSIGNED_CONTEXT ( ( #4528, #4383, #2880 ) ) REPRESENTATION_CONTEXT ( 'NONE', 'WORKASPACE' ) );
#2197 = AXIS2_PLACEMENT_3D ( 'NONE', #9707, #7436, #2934 ) ;
#2198 = DIRECTION ( 'NONE',  ( -0.3286710990610922090, -6.289316826390952918E-29, -0.9444444444444435316 ) ) ;
#2199 = CARTESIAN_POINT ( 'NONE',  ( -5.562309845534701758, 60.99999999999999289, 37.56426808735052703 ) ) ;
#2200 = ORIENTED_EDGE ( 'NONE', *, *, #9573, .T. ) ;
#2201 = CARTESIAN_POINT ( 'NONE',  ( 9.350174078884196049, -0.2661211825927956576, 41.70529496454247464 ) ) ;
#2202 = APPLICATION_PROTOCOL_DEFINITION ( 'draft international standard', 'automotive_design', 1998, #3923 ) ;
#2203 = AXIS2_PLACEMENT_3D ( 'NONE', #8656, #1878, #2114 ) ;
#2204 = VERTEX_POINT ( 'NONE', #2 ) ;
#2205 = DIRECTION ( 'NONE',  ( -1.820952055660014662E-28, -1.000000000000000000, -7.038118388768679669E-30 ) ) ;
#2206 = ORIENTED_EDGE ( 'NONE', *, *, #1473, .T. ) ;
#2207 = LINE ( 'NONE', #9739, #4190 ) ;
#2208 = VERTEX_POINT ( 'NONE', #6741 ) ;
#2209 = PLANE ( 'NONE',  #5620 ) ;
#2210 = VERTEX_POINT ( 'NONE', #9035 ) ;
#2211 = CARTESIAN_POINT ( 'NONE',  ( -4.149849522310169903, 12.39897866860190767, 43.55983959218083612 ) ) ;
#2212 = PLANE ( 'NONE',  #1452 ) ;
#2213 = DIRECTION ( 'NONE',  ( 0.000000000000000000, -1.000000000000000000, 0.000000000000000000 ) ) ;
#2214 = AXIS2_PLACEMENT_3D ( 'NONE', #1430, #8841, #8010 ) ;
#2215 = VECTOR ( 'NONE', #2887, 1000.000000000000000 ) ;
#2216 = ORIENTED_EDGE ( 'NONE', *, *, #3039, .T. ) ;
#2217 = CARTESIAN_POINT ( 'NONE',  ( -5.987883466156522339, 58.97190912209828895, 35.53684633323566544 ) ) ;
#2218 = ORIENTED_EDGE ( 'NONE', *, *, #4260, .T. ) ;
#2219 = ORIENTED_EDGE ( 'NONE', *, *, #8815, .T. ) ;
#2220 = CARTESIAN_POINT ( 'NONE',  ( 6.000000000000001776, 28.28385863652523824, -30.12488991936162108 ) ) ;
#2221 = CARTESIAN_POINT ( 'NONE',  ( 12.20000000000000107, 2.210487472460972698E-16, -1.610000000000000098 ) ) ;
#2222 = DIRECTION ( 'NONE',  ( 0.001963426291157480824, 0.9999980724767419948, 0.000000000000000000 ) ) ;
#2223 = AXIS2_PLACEMENT_3D ( 'NONE', #5491, #3350, #1723 ) ;
#2224 = CARTESIAN_POINT ( 'NONE',  ( -8.216777476527274970, 78.08723716182652197, -23.61111111111111427 ) ) ;
#2225 = CONICAL_SURFACE ( 'NONE', #7765, 26.00000000000000355, 0.7853981633974346233 ) ;
#2226 = DIRECTION ( 'NONE',  ( 0.000000000000000000, -0.000000000000000000, 1.000000000000000000 ) ) ;
#2227 = VECTOR ( 'NONE', #5231, 1000.000000000000000 ) ;
#2228 = ORIENTED_EDGE ( 'NONE', *, *, #9343, .T. ) ;
#2229 = EDGE_CURVE ( 'NONE', #8766, #7406, #3059, .T. ) ;
#2230 = CYLINDRICAL_SURFACE ( 'NONE', #9711, 1.500000000000003109 ) ;
#2231 = EDGE_CURVE ( 'NONE', #7884, #2072, #5899, .T. ) ;
#2232 = DIRECTION ( 'NONE',  ( -1.000000000000000000, 0.000000000000000000, 0.000000000000000000 ) ) ;
#2233 = CARTESIAN_POINT ( 'NONE',  ( 1.555535097482682654E-26, 78.08723716182652197, -25.00000000000000000 ) ) ;
#2234 = CARTESIAN_POINT ( 'NONE',  ( -10.00000000000001599, 3.294852476641298100, 300.0000000000000000 ) ) ;
#2235 = FILL_AREA_STYLE ('',( #3789 ) ) ;
#2236 = VERTEX_POINT ( 'NONE', #6845 ) ;
#2237 = DIRECTION ( 'NONE',  ( -0.000000000000000000, -1.000000000000000000, -0.000000000000000000 ) ) ;
#2238 = VECTOR ( 'NONE', #3063, 1000.000000000000341 ) ;
#2239 = EDGE_CURVE ( 'NONE', #8213, #8367, #1649, .T. ) ;
#2240 = EDGE_CURVE ( 'NONE', #9175, #8122, #2898, .T. ) ;
#2241 = AXIS2_PLACEMENT_3D ( 'NONE', #687, #1282, #4297 ) ;
#2242 = ADVANCED_FACE ( 'NONE', ( #8190 ), #738, .F. ) ;
#2243 = CARTESIAN_POINT ( 'NONE',  ( 0.000000000000000000, -15.00000000000000000, 0.000000000000000000 ) ) ;
#2244 = VERTEX_POINT ( 'NONE', #6052 ) ;
#2245 = CARTESIAN_POINT ( 'NONE',  ( 34.07933880998927378, 61.99999999999999289, -5.371095444502794081 ) ) ;
#2246 = CARTESIAN_POINT ( 'NONE',  ( 0.4484383372385683519, -15.00000000000000000, 30.56042761519584872 ) ) ;
#2247 = ORIENTED_EDGE ( 'NONE', *, *, #2427, .F. ) ;
#2248 = EDGE_CURVE ( 'NONE', #1081, #9622, #689, .T. ) ;
#2249 = EDGE_CURVE ( 'NONE', #8507, #3257, #2892, .T. ) ;
#2250 = CARTESIAN_POINT ( 'NONE',  ( 26.32489316217636954, -15.00000000000000000, 6.000000000000000000 ) ) ;
#2251 = EDGE_CURVE ( 'NONE', #7059, #7114, #6000, .T. ) ;
#2252 = CIRCLE ( 'NONE', #8902, 26.00000000000000355 ) ;
#2253 = CARTESIAN_POINT ( 'NONE',  ( 5.134502662544400131, 61.85904243767787847, -37.56426808735048439 ) ) ;
#2254 = ORIENTED_EDGE ( 'NONE', *, *, #3166, .T. ) ;
#2255 = EDGE_CURVE ( 'NONE', #167, #2517, #1796, .T. ) ;
#2256 = CARTESIAN_POINT ( 'NONE',  ( 12.43148144571613223, -2.046608012193396942, 36.96605690027389102 ) ) ;
#2257 = PRODUCT_CONTEXT ( 'NONE', #6297, 'mechanical' ) ;
#2258 = AXIS2_PLACEMENT_3D ( 'NONE', #1165, #3524, #8721 ) ;
#2259 = ORIENTED_EDGE ( 'NONE', *, *, #2546, .F. ) ;
#2260 = CARTESIAN_POINT ( 'NONE',  ( -26.32489316217636954, -15.00000000000000000, 6.000000000000009770 ) ) ;
#2261 = CIRCLE ( 'NONE', #7323, 31.49999999999999289 ) ;
#2262 = CARTESIAN_POINT ( 'NONE',  ( 0.000000000000000000, 59.99999999999999289, 0.000000000000000000 ) ) ;
#2263 = CARTESIAN_POINT ( 'NONE',  ( 1.084683744678891232E-26, 56.00000000000030553, -26.00000000000003197 ) ) ;
#2264 = ORIENTED_EDGE ( 'NONE', *, *, #8365, .F. ) ;
#2265 = DIRECTION ( 'NONE',  ( -0.000000000000000000, -0.000000000000000000, 1.000000000000000000 ) ) ;
#2266 = AXIS2_PLACEMENT_3D ( 'NONE', #3694, #2947, #2190 ) ;
#2267 = VERTEX_POINT ( 'NONE', #6107 ) ;
#2268 = CARTESIAN_POINT ( 'NONE',  ( -1.306712379120655632, 13.21469178175683190, 43.95913021330854065 ) ) ;
#2269 = DIRECTION ( 'NONE',  ( -1.000000000000000000, -0.000000000000000000, -0.000000000000000000 ) ) ;
#2270 = DIRECTION ( 'NONE',  ( 0.000000000000000000, 1.000000000000000000, -0.000000000000000000 ) ) ;
#2271 = VECTOR ( 'NONE', #4850, 1000.000000000000000 ) ;
#2272 = EDGE_LOOP ( 'NONE', ( #2565, #2344 ) ) ;
#2273 = CARTESIAN_POINT ( 'NONE',  ( 5.562309845534932684, 60.99999999999999289, -33.06426808735049150 ) ) ;
#2274 = EDGE_LOOP ( 'NONE', ( #2478, #1343, #853, #4650 ) ) ;
#2275 = AXIS2_PLACEMENT_3D ( 'NONE', #9603, #8765, #2035 ) ;
#2276 = EDGE_CURVE ( 'NONE', #2374, #915, #7159, .T. ) ;
#2277 = UNCERTAINTY_MEASURE_WITH_UNIT (LENGTH_MEASURE( 1.000000000000000082E-05 ), #147, 'distance_accuracy_value', 'NONE');
#2278 = TOROIDAL_SURFACE ( 'NONE', #5907, 37.00000000000000711, 1.000000000000000888 ) ;
#2279 = ORIENTED_EDGE ( 'NONE', *, *, #3349, .T. ) ;
#2280 = DIRECTION ( 'NONE',  ( 0.000000000000000000, -1.000000000000000000, 0.000000000000000000 ) ) ;
#2281 = CARTESIAN_POINT ( 'NONE',  ( -0.02610464500743471528, -11.70511861050984947, 38.99999126342864741 ) ) ;
#2282 = LINE ( 'NONE', #5316, #2435 ) ;
#2283 = CARTESIAN_POINT ( 'NONE',  ( 5.000171879512024908, -8.491196122513333222, 39.08124479469799439 ) ) ;
#2284 = CIRCLE ( 'NONE', #1974, 17.99999999999999645 ) ;
#2285 = VECTOR ( 'NONE', #9290, 1000.000000000000114 ) ;
#2286 = AXIS2_PLACEMENT_3D ( 'NONE', #7474, #4416, #2967 ) ;
#2287 = ORIENTED_EDGE ( 'NONE', *, *, #7774, .T. ) ;
#2288 = CARTESIAN_POINT ( 'NONE',  ( -10.84614626901596601, 59.99999999999999289, -31.16666666666667851 ) ) ;
#2289 = CARTESIAN_POINT ( 'NONE',  ( -4.861949598180842713, 59.13521925290943670, 35.48792514263537612 ) ) ;
#2290 = ORIENTED_EDGE ( 'NONE', *, *, #4810, .F. ) ;
#2291 = DIRECTION ( 'NONE',  ( -0.000000000000000000, -1.000000000000000000, -0.000000000000000000 ) ) ;
#2292 = DIRECTION ( 'NONE',  ( 0.000000000000000000, 0.000000000000000000, 1.000000000000000000 ) ) ;
#2293 = LINE ( 'NONE', #6833, #1351 ) ;
#2294 = VECTOR ( 'NONE', #5837, 1000.000000000000000 ) ;
#2295 = FACE_OUTER_BOUND ( 'NONE', #5394, .T. ) ;
#2296 = SURFACE_SIDE_STYLE ('',( #833 ) ) ;
#2297 = PLANE ( 'NONE',  #1122 ) ;
#2298 = VERTEX_POINT ( 'NONE', #5332 ) ;
#2299 = DIRECTION ( 'NONE',  ( 0.000000000000000000, 1.000000000000000000, 0.000000000000000000 ) ) ;
#2300 = ADVANCED_FACE ( 'NONE', ( #840 ), #6694, .T. ) ;
#2301 = AXIS2_PLACEMENT_3D ( 'NONE', #3294, #4841, #6257 ) ;
#2302 = DIRECTION ( 'NONE',  ( -1.735493991486225972E-29, 6.508102468073347395E-30, 1.000000000000000000 ) ) ;
#2303 = FACE_OUTER_BOUND ( 'NONE', #5668, .T. ) ;
#2304 = ORIENTED_EDGE ( 'NONE', *, *, #5533, .F. ) ;
#2305 = LINE ( 'NONE', #8984, #374 ) ;
#2306 = CARTESIAN_POINT ( 'NONE',  ( 6.332203200428770273, -7.897660556950563127, 38.80169624000574657 ) ) ;
#2307 = ORIENTED_EDGE ( 'NONE', *, *, #5529, .F. ) ;
#2308 = CYLINDRICAL_SURFACE ( 'NONE', #9506, 1.500000000000001332 ) ;
#2309 = DIRECTION ( 'NONE',  ( -0.000000000000000000, 0.5000000000000002220, -0.8660254037844384856 ) ) ;
#2310 = EDGE_LOOP ( 'NONE', ( #7054, #6754 ) ) ;
#2311 = CARTESIAN_POINT ( 'NONE',  ( 9.194894985997349224, -0.6766425519222662999, 38.05435396104630996 ) ) ;
#2312 = ORIENTED_EDGE ( 'NONE', *, *, #7743, .F. ) ;
#2313 = DIRECTION ( 'NONE',  ( 1.735493991486225972E-29, -6.508102468073347395E-30, -1.000000000000000000 ) ) ;
#2314 = ADVANCED_FACE ( 'NONE', ( #2303 ), #8291, .T. ) ;
#2315 = DIRECTION ( 'NONE',  ( 0.3286710990610906546, 0.000000000000000000, 0.9444444444444440867 ) ) ;
#2316 = CARTESIAN_POINT ( 'NONE',  ( 0.000000000000000000, 0.000000000000000000, 0.000000000000000000 ) ) ;
#2317 = EDGE_CURVE ( 'NONE', #7738, #1992, #5896, .T. ) ;
#2318 = ORIENTED_EDGE ( 'NONE', *, *, #7337, .T. ) ;
#2319 = DIRECTION ( 'NONE',  ( -0.3286710990610922090, -6.289316826390952918E-29, -0.9444444444444435316 ) ) ;
#2320 = EDGE_CURVE ( 'NONE', #9368, #6765, #2252, .T. ) ;
#2321 = ORIENTED_EDGE ( 'NONE', *, *, #9459, .T. ) ;
#2322 = CARTESIAN_POINT ( 'NONE',  ( -2.620222824297394393, 12.96846514759271152, 43.83512211430772965 ) ) ;
#2323 = B_SPLINE_CURVE_WITH_KNOTS ( 'NONE', 3,
 ( #8977, #6686, #9721, #1460 ),
 .UNSPECIFIED., .F., .F.,
 ( 4, 4 ),
 ( 9.813077866773594792E-18, 0.003679109433542027217 ),
 .UNSPECIFIED. ) ;
#2324 = DIRECTION ( 'NONE',  ( 0.000000000000000000, -0.000000000000000000, 1.000000000000000000 ) ) ;
#2325 = CARTESIAN_POINT ( 'NONE',  ( -9.351925007598564932, -0.2614073996901185026, 41.70440666569142252 ) ) ;
#2326 = ORIENTED_EDGE ( 'NONE', *, *, #4204, .F. ) ;
#2327 = CARTESIAN_POINT ( 'NONE',  ( 9.860132971832495485, 39.99999999999999289, 28.33333333333341031 ) ) ;
#2328 = CARTESIAN_POINT ( 'NONE',  ( -4.000000000000001776, 0.000000000000000000, 4.336808689942015271E-16 ) ) ;
#2329 = EDGE_CURVE ( 'NONE', #1005, #5592, #4652, .T. ) ;
#2330 = VERTEX_POINT ( 'NONE', #5229 ) ;
#2331 = ORIENTED_EDGE ( 'NONE', *, *, #7093, .F. ) ;
#2332 = CYLINDRICAL_SURFACE ( 'NONE', #2582, 4.500000000000003553 ) ;
#2333 = CARTESIAN_POINT ( 'NONE',  ( 1.300000000000000044, 0.000000000000000000, 1.249999999999999778 ) ) ;
#2334 = CARTESIAN_POINT ( 'NONE',  ( 6.000000000000007994, 30.00000000000000000, 26.32489316217636954 ) ) ;
#2335 = ORIENTED_EDGE ( 'NONE', *, *, #1978, .F. ) ;
#2336 = CARTESIAN_POINT ( 'NONE',  ( -33.06426808735054124, 59.99576382555915899, -3.062309845534580077 ) ) ;
#2337 = DIRECTION ( 'NONE',  ( -1.000000000000000000, 0.000000000000000000, 0.000000000000000000 ) ) ;
#2338 = VERTEX_POINT ( 'NONE', #152 ) ;
#2339 = DIRECTION ( 'NONE',  ( 0.000000000000000000, 0.000000000000000000, 1.000000000000000000 ) ) ;
#2340 = CARTESIAN_POINT ( 'NONE',  ( 3.619905045646671926, 59.65318172148984388, -34.64718077370495308 ) ) ;
#2341 = LINE ( 'NONE', #2234, #8706 ) ;
#2342 = DIRECTION ( 'NONE',  ( -0.9860132971832694659, -1.788557213313974350E-28, 0.1666666666666658247 ) ) ;
#2343 = CARTESIAN_POINT ( 'NONE',  ( 1.300000000000000044, 0.7216878364870328300, -1.250000000000000000 ) ) ;
#2344 = ORIENTED_EDGE ( 'NONE', *, *, #169, .F. ) ;
#2345 = CARTESIAN_POINT ( 'NONE',  ( -8.216777476527274970, 48.50000000000033396, -23.61111111111111427 ) ) ;
#2346 = VECTOR ( 'NONE', #5667, 1000.000000000000000 ) ;
#2347 = AXIS2_PLACEMENT_3D ( 'NONE', #8029, #1265, #6535 ) ;
#2348 = DIRECTION ( 'NONE',  ( 0.000000000000000000, 1.000000000000000000, 0.000000000000000000 ) ) ;
#2349 = AXIS2_PLACEMENT_3D ( 'NONE', #7819, #1785, #7766 ) ;
#2350 = PRODUCT ( 'socket button head screw_iso_ISO 7380 - M4 x 10 - 10N', 'socket button head screw_iso_ISO 7380 - M4 x 10 - 10N', '', ( #9735 ) ) ;
#2351 = VERTEX_POINT ( 'NONE', #9371 ) ;
#2352 = CARTESIAN_POINT ( 'NONE',  ( 29.00000000000000355, 28.99999999999997158, -4.000000000000007105 ) ) ;
#2353 = CARTESIAN_POINT ( 'NONE',  ( 8.119362783942410289, -15.00000000000000000, 36.91696022903513352 ) ) ;
#2354 = ORIENTED_EDGE ( 'NONE', *, *, #5037, .T. ) ;
#2355 = CARTESIAN_POINT ( 'NONE',  ( 5.562309845534588959, 59.99999999999999289, -33.06426808735054124 ) ) ;
#2356 = VECTOR ( 'NONE', #2178, 1000.000000000000341 ) ;
#2357 = CARTESIAN_POINT ( 'NONE',  ( -33.06426808735054124, 49.99999999999999289, -5.562309845534581854 ) ) ;
#2358 = VERTEX_POINT ( 'NONE', #3994 ) ;
#2359 = ORIENTED_EDGE ( 'NONE', *, *, #5778, .T. ) ;
#2360 = DIRECTION ( 'NONE',  ( -0.000000000000000000, 1.000000000000000000, -0.000000000000000000 ) ) ;
#2361 = VECTOR ( 'NONE', #5255, 1000.000000000000000 ) ;
#2362 = DIRECTION ( 'NONE',  ( -0.000000000000000000, 0.000000000000000000, -1.000000000000000000 ) ) ;
#2363 = CARTESIAN_POINT ( 'NONE',  ( 6.000000000000007994, 30.00000000000000000, 28.37252191822215863 ) ) ;
#2364 = ORIENTED_EDGE ( 'NONE', *, *, #9216, .F. ) ;
#2365 = CARTESIAN_POINT ( 'NONE',  ( -0.02206928620401079830, -9.470079073673241865, 39.52734620791224529 ) ) ;
#2366 = VECTOR ( 'NONE', #44, 1000.000000000000000 ) ;
#2367 = ORIENTED_EDGE ( 'NONE', *, *, #1249, .F. ) ;
#2368 = DIRECTION ( 'NONE',  ( 0.000000000000000000, 0.000000000000000000, 1.000000000000000000 ) ) ;
#2369 = CARTESIAN_POINT ( 'NONE',  ( 24.67792535850613334, 28.99999999999997158, -4.000000000000006217 ) ) ;
#2370 = DIRECTION ( 'NONE',  ( 0.000000000000000000, 0.000000000000000000, -1.000000000000000000 ) ) ;
#2371 = EDGE_CURVE ( 'NONE', #22, #8061, #9690, .T. ) ;
#2372 = EDGE_CURVE ( 'NONE', #1467, #3887, #5524, .T. ) ;
#2373 = EDGE_CURVE ( 'NONE', #7030, #1931, #1675, .T. ) ;
#2374 = VERTEX_POINT ( 'NONE', #7793 ) ;
#2375 = CARTESIAN_POINT ( 'NONE',  ( 32.92587516511807166, 59.99999999999999289, 3.065181147996828948 ) ) ;
#2376 = VERTEX_POINT ( 'NONE', #295 ) ;
#2377 = ORIENTED_EDGE ( 'NONE', *, *, #5999, .T. ) ;
#2378 = AXIS2_PLACEMENT_3D ( 'NONE', #3582, #9680, #8304 ) ;
#2379 = PLANE ( 'NONE',  #4488 ) ;
#2380 = DIRECTION ( 'NONE',  ( 0.000000000000000000, 0.000000000000000000, 1.000000000000000000 ) ) ;
#2381 = VECTOR ( 'NONE', #9273, 1000.000000000000114 ) ;
#2382 = CARTESIAN_POINT ( 'NONE',  ( 16.70299909897254409, 60.99999999999999289, -30.18708036726510002 ) ) ;
#2383 = ADVANCED_FACE ( 'NONE', ( #4787 ), #8533, .F. ) ;
#2384 = EDGE_CURVE ( 'NONE', #7811, #3246, #2890, .T. ) ;
#2385 = ORIENTED_EDGE ( 'NONE', *, *, #3424, .T. ) ;
#2386 = CARTESIAN_POINT ( 'NONE',  ( -8.545448575588387996, 47.00000000000034106, -24.55555555555564240 ) ) ;
#2387 = LINE ( 'NONE', #1654, #6606 ) ;
#2388 = CARTESIAN_POINT ( 'NONE',  ( -3.339929591309179990, 59.80724097760847968, 34.22175998453048607 ) ) ;
#2389 = ORIENTED_EDGE ( 'NONE', *, *, #4010, .F. ) ;
#2390 = CARTESIAN_POINT ( 'NONE',  ( -38.00000000000000711, 39.99999999999999289, -3.980288726281173287E-13 ) ) ;
#2391 = VECTOR ( 'NONE', #7363, 1000.000000000000000 ) ;
#2392 = CARTESIAN_POINT ( 'NONE',  ( 6.597235312685898911, 59.03111057313396515, -35.34929737147491835 ) ) ;
#2393 = DIRECTION ( 'NONE',  ( 0.000000000000000000, 1.000000000000000000, 0.000000000000000000 ) ) ;
#2394 = DIRECTION ( 'NONE',  ( 0.000000000000000000, 0.000000000000000000, -1.000000000000000000 ) ) ;
#2395 = FACE_OUTER_BOUND ( 'NONE', #656, .T. ) ;
#2396 = VERTEX_POINT ( 'NONE', #1860 ) ;
#2397 = DIRECTION ( 'NONE',  ( -0.000000000000000000, -1.000000000000000000, -0.000000000000000000 ) ) ;
#2398 = CIRCLE ( 'NONE', #5866, 5.000000000000004441 ) ;
#2399 = DIRECTION ( 'NONE',  ( 1.735493991486225972E-29, -6.508102468073347395E-30, -1.000000000000000000 ) ) ;
#2400 = ORIENTED_EDGE ( 'NONE', *, *, #41, .T. ) ;
#2401 = DIRECTION ( 'NONE',  ( 0.3286710990610922090, 6.289316826390952918E-29, 0.9444444444444435316 ) ) ;
#2402 = CARTESIAN_POINT ( 'NONE',  ( 4.000000000000008882, 0.000000000000000000, 29.00000000000000355 ) ) ;
#2403 = ADVANCED_FACE ( 'NONE', ( #931 ), #7483, .F. ) ;
#2404 = CIRCLE ( 'NONE', #7938, 26.00000000000015987 ) ;
#2405 = VERTEX_POINT ( 'NONE', #3903 ) ;
#2406 = DIRECTION ( 'NONE',  ( 1.047444401652940795E-14, 0.000000000000000000, -1.000000000000000000 ) ) ;
#2407 = DIRECTION ( 'NONE',  ( 0.000000000000000000, -1.000000000000000000, 0.000000000000000000 ) ) ;
#2408 = VERTEX_POINT ( 'NONE', #1761 ) ;
#2409 = CARTESIAN_POINT ( 'NONE',  ( 3.017393985291145331, -6.258907930525880126, 38.92018111626612864 ) ) ;
#2410 = DIRECTION ( 'NONE',  ( 0.000000000000000000, 0.000000000000000000, 1.000000000000000000 ) ) ;
#2411 = DIRECTION ( 'NONE',  ( 0.000000000000000000, 0.000000000000000000, -1.000000000000000000 ) ) ;
#2412 = DIRECTION ( 'NONE',  ( 0.000000000000000000, 0.000000000000000000, -1.000000000000000000 ) ) ;
#2413 = DIRECTION ( 'NONE',  ( 0.000000000000000000, 0.000000000000000000, -1.000000000000000000 ) ) ;
#2414 = ORIENTED_EDGE ( 'NONE', *, *, #2084, .T. ) ;
#2415 = FACE_OUTER_BOUND ( 'NONE', #2610, .T. ) ;
#2416 = CARTESIAN_POINT ( 'NONE',  ( 1.040310318760209318E-26, 47.50000000000033396, -25.00000000000000000 ) ) ;
#2417 = CIRCLE ( 'NONE', #7954, 2.500000000000002220 ) ;
#2418 = ADVANCED_FACE ( 'NONE', ( #7039 ), #4838, .T. ) ;
#2419 = CIRCLE ( 'NONE', #76, 1.500000000000001332 ) ;
#2420 = ORIENTED_EDGE ( 'NONE', *, *, #4308, .F. ) ;
#2421 = VERTEX_POINT ( 'NONE', #3290 ) ;
#2422 = CARTESIAN_POINT ( 'NONE',  ( 0.000000000000000000, 59.99999999999999289, 0.000000000000000000 ) ) ;
#2423 = EDGE_LOOP ( 'NONE', ( #5063, #9323, #1190 ) ) ;
#2424 = EDGE_CURVE ( 'NONE', #5694, #2645, #6300, .T. ) ;
#2425 = ORIENTED_EDGE ( 'NONE', *, *, #6649, .F. ) ;
#2426 = CARTESIAN_POINT ( 'NONE',  ( -3.886469093799143071, -5.959786720418388306, 38.86437971944521053 ) ) ;
#2427 = EDGE_CURVE ( 'NONE', #9170, #3565, #4334, .T. ) ;
#2428 = CARTESIAN_POINT ( 'NONE',  ( 0.000000000000000000, 39.99999999999999289, 0.000000000000000000 ) ) ;
#2429 = AXIS2_PLACEMENT_3D ( 'NONE', #3061, #6080, #1488 ) ;
#2430 = DIRECTION ( 'NONE',  ( 0.000000000000000000, 0.000000000000000000, 1.000000000000000000 ) ) ;
#2431 = EDGE_LOOP ( 'NONE', ( #7002, #7017, #9351, #1046, #3990, #9415 ) ) ;
#2432 = DIRECTION ( 'NONE',  ( -0.000000000000000000, 1.000000000000000000, -0.000000000000000000 ) ) ;
#2433 = FACE_OUTER_BOUND ( 'NONE', #5913, .T. ) ;
#2434 = AXIS2_PLACEMENT_3D ( 'NONE', #1777, #1044, #5681 ) ;
#2435 = VECTOR ( 'NONE', #8326, 999.9999999999998863 ) ;
#2436 = ORIENTED_EDGE ( 'NONE', *, *, #2546, .T. ) ;
#2437 = CARTESIAN_POINT ( 'NONE',  ( 9.815840903884561541, 59.99999999999999289, -28.34870838944214100 ) ) ;
#2438 = CARTESIAN_POINT ( 'NONE',  ( 3.055999436386200419, 59.99999999999998579, -33.03613408327221634 ) ) ;
#2439 = ADVANCED_FACE ( 'NONE', ( #2450 ), #5484, .F. ) ;
#2440 = CARTESIAN_POINT ( 'NONE',  ( -28.33333333333344939, 39.99999999999999289, 9.860132971832396009 ) ) ;
#2441 = EDGE_CURVE ( 'NONE', #6423, #9611, #8638, .T. ) ;
#2442 = DIRECTION ( 'NONE',  ( 1.735493991486225972E-29, -6.508102468073347395E-30, -1.000000000000000000 ) ) ;
#2443 = VERTEX_POINT ( 'NONE', #6155 ) ;
#2444 = EDGE_CURVE ( 'NONE', #7011, #3069, #1027, .T. ) ;
#2445 = DIRECTION ( 'NONE',  ( 0.000000000000000000, -1.000000000000000000, 0.000000000000000000 ) ) ;
#2446 = AXIS2_PLACEMENT_3D ( 'NONE', #272, #3261, #9298 ) ;
#2447 = VECTOR ( 'NONE', #94, 1000.000000000000000 ) ;
#2448 = AXIS2_PLACEMENT_3D ( 'NONE', #1107, #7122, #4077 ) ;
#2449 = VECTOR ( 'NONE', #6864, 1000.000000000000227 ) ;
#2450 = FACE_OUTER_BOUND ( 'NONE', #3947, .T. ) ;
#2451 = EDGE_CURVE ( 'NONE', #5638, #478, #6208, .T. ) ;
#2452 = ORIENTED_EDGE ( 'NONE', *, *, #1988, .T. ) ;
#2453 = DIRECTION ( 'NONE',  ( 0.000000000000000000, 0.000000000000000000, -1.000000000000000000 ) ) ;
#2454 = CARTESIAN_POINT ( 'NONE',  ( -5.562309845534584518, 59.99999999999999289, 30.56426808735054124 ) ) ;
#2455 = ORIENTED_EDGE ( 'NONE', *, *, #3473, .T. ) ;
#2456 = DIRECTION ( 'NONE',  ( -1.820952055660014662E-28, -1.000000000000000000, -7.038118388768679669E-30 ) ) ;
#2457 = COLOUR_RGB ( '',0.7921568627450980005, 0.8196078431372548767, 0.9333333333333333481 ) ;
#2458 = CARTESIAN_POINT ( 'NONE',  ( 4.716066576642940156, 61.89689025924450050, -37.50432491070253604 ) ) ;
#2459 = ORIENTED_EDGE ( 'NONE', *, *, #690, .F. ) ;
#2460 = LINE ( 'NONE', #5494, #1737 ) ;
#2461 = DIRECTION ( 'NONE',  ( 0.000000000000000000, 1.000000000000000000, 0.000000000000000000 ) ) ;
#2462 = EDGE_LOOP ( 'NONE', ( #5183, #8086, #2663, #1323 ) ) ;
#2463 = DIRECTION ( 'NONE',  ( -0.000000000000000000, 0.5000000000000002220, -0.8660254037844384856 ) ) ;
#2464 = LINE ( 'NONE', #5498, #2936 ) ;
#2465 = ORIENTED_EDGE ( 'NONE', *, *, #3112, .T. ) ;
#2466 = DIRECTION ( 'NONE',  ( 0.9449569463147371451, -0.000000000000000000, 0.3271946967961539832 ) ) ;
#2467 = CARTESIAN_POINT ( 'NONE',  ( -3.270419483466965982, -6.161042622928358803, 43.72827664804632519 ) ) ;
#2468 = ORIENTED_EDGE ( 'NONE', *, *, #2534, .T. ) ;
#2469 = CARTESIAN_POINT ( 'NONE',  ( -34.16461100076188018, 59.56421283147439283, -7.812829873186591279 ) ) ;
#2470 = ORIENTED_EDGE ( 'NONE', *, *, #7272, .F. ) ;
#2471 = DIRECTION ( 'NONE',  ( 1.735493991486225972E-29, -6.508102468073347395E-30, -1.000000000000000000 ) ) ;
#2472 = ORIENTED_EDGE ( 'NONE', *, *, #2805, .T. ) ;
#2473 = ORIENTED_EDGE ( 'NONE', *, *, #5704, .F. ) ;
#2474 = CARTESIAN_POINT ( 'NONE',  ( -7.065584702402819772, -3.825344972707461100, 38.47648702749351912 ) ) ;
#2475 = DIRECTION ( 'NONE',  ( 0.000000000000000000, 0.000000000000000000, 1.000000000000000000 ) ) ;
#2476 = CARTESIAN_POINT ( 'NONE',  ( 1.030449557444946671E-26, 53.00000000000031974, -26.00000000000006395 ) ) ;
#2477 = EDGE_CURVE ( 'NONE', #8414, #903, #7792, .T. ) ;
#2478 = ORIENTED_EDGE ( 'NONE', *, *, #411, .T. ) ;
#2479 = DIRECTION ( 'NONE',  ( 0.6195972517514871658, 0.000000000000000000, 0.7849198975831892522 ) ) ;
#2480 = ORIENTED_EDGE ( 'NONE', *, *, #8731, .F. ) ;
#2481 = DIRECTION ( 'NONE',  ( 0.000000000000000000, 0.000000000000000000, 1.000000000000000000 ) ) ;
#2482 = CARTESIAN_POINT ( 'NONE',  ( 4.249163891373067159, 59.35847319192267690, -35.19820543205469221 ) ) ;
#2483 = CARTESIAN_POINT ( 'NONE',  ( -31.00000000000000711, -10.00000000000000533, 6.000000000000009770 ) ) ;
#2484 = FACE_OUTER_BOUND ( 'NONE', #9071, .T. ) ;
#2485 = CARTESIAN_POINT ( 'NONE',  ( 1.555535097482682654E-26, 78.08723716182652197, -25.00000000000000000 ) ) ;
#2486 = EDGE_CURVE ( 'NONE', #5205, #3216, #8439, .T. ) ;
#2487 = EDGE_CURVE ( 'NONE', #4270, #9611, #6368, .T. ) ;
#2488 = EDGE_CURVE ( 'NONE', #4231, #6406, #3393, .T. ) ;
#2489 = DIRECTION ( 'NONE',  ( 0.000000000000000000, -1.000000000000000000, 0.000000000000000000 ) ) ;
#2490 = DIRECTION ( 'NONE',  ( 0.9444444444444403119, 0.000000000000000000, -0.3286710990611015903 ) ) ;
#2491 = ORIENTED_EDGE ( 'NONE', *, *, #9609, .F. ) ;
#2492 = CARTESIAN_POINT ( 'NONE',  ( 8.106025752690735331, 61.92736406916336733, -36.79170325027448030 ) ) ;
#2493 = DIRECTION ( 'NONE',  ( 0.000000000000000000, 0.000000000000000000, 1.000000000000000000 ) ) ;
#2494 = ORIENTED_EDGE ( 'NONE', *, *, #8267, .T. ) ;
#2495 = DIRECTION ( 'NONE',  ( 0.000000000000000000, 1.000000000000000000, 0.000000000000000000 ) ) ;
#2496 = DIRECTION ( 'NONE',  ( 0.000000000000000000, 0.000000000000000000, 1.000000000000000000 ) ) ;
#2497 = ADVANCED_FACE ( 'NONE', ( #4146 ), #2049, .F. ) ;
#2498 = AXIS2_PLACEMENT_3D ( 'NONE', #67, #2362, #5396 ) ;
#2499 = CARTESIAN_POINT ( 'NONE',  ( 4.404177573089986808, -5.731393103011397372, 38.82088277608229276 ) ) ;
#2500 = EDGE_CURVE ( 'NONE', #344, #2516, #1129, .T. ) ;
#2501 = DIRECTION ( 'NONE',  ( -0.7849198975831888081, 0.000000000000000000, 0.6195972517514876099 ) ) ;
#2502 = ORIENTED_EDGE ( 'NONE', *, *, #6659, .T. ) ;
#2503 = DIRECTION ( 'NONE',  ( 0.000000000000000000, 1.000000000000000000, 0.000000000000000000 ) ) ;
#2504 = EDGE_LOOP ( 'NONE', ( #8119, #8136, #5007, #6177 ) ) ;
#2505 = CARTESIAN_POINT ( 'NONE',  ( -8.545448575588384443, 48.50000000000033396, -24.55555555555566727 ) ) ;
#2506 = ORIENTED_EDGE ( 'NONE', *, *, #749, .T. ) ;
#2507 = VECTOR ( 'NONE', #6731, 1000.000000000000227 ) ;
#2508 = CARTESIAN_POINT ( 'NONE',  ( 31.00000000000000711, 27.42469319230601243, 6.000000000000000000 ) ) ;
#2509 = CARTESIAN_POINT ( 'NONE',  ( 4.000000000000001776, 0.000000000000000000, -24.67792535850613334 ) ) ;
#2510 = LINE ( 'NONE', #4069, #5366 ) ;
#2511 = CIRCLE ( 'NONE', #333, 2.499999999999998668 ) ;
#2512 = ORIENTED_EDGE ( 'NONE', *, *, #930, .F. ) ;
#2513 = CARTESIAN_POINT ( 'NONE',  ( -35.56420151578587507, 58.98289357006406419, -5.732470078048709894 ) ) ;
#2514 = ORIENTED_EDGE ( 'NONE', *, *, #2451, .F. ) ;
#2515 = CARTESIAN_POINT ( 'NONE',  ( 28.33333333333337833, 59.99999999999999289, -9.860132971832594961 ) ) ;
#2516 = VERTEX_POINT ( 'NONE', #4195 ) ;
#2517 = VERTEX_POINT ( 'NONE', #9519 ) ;
#2518 = CARTESIAN_POINT ( 'NONE',  ( -9.982669663254970516, 3.970470032139787442, 41.37368756539773074 ) ) ;
#2519 = EDGE_CURVE ( 'NONE', #8611, #9175, #2419, .T. ) ;
#2520 = PLANE ( 'NONE',  #2448 ) ;
#2521 = AXIS2_PLACEMENT_3D ( 'NONE', #331, #2531, #2394 ) ;
#2522 = CYLINDRICAL_SURFACE ( 'NONE', #7780, 2.500000000000002220 ) ;
#2523 = ADVANCED_FACE ( 'NONE', ( #5670 ), #7897, .T. ) ;
#2524 = ORIENTED_EDGE ( 'NONE', *, *, #668, .T. ) ;
#2525 = LINE ( 'NONE', #6433, #951 ) ;
#2526 = VECTOR ( 'NONE', #1753, 1000.000000000000000 ) ;
#2527 = ORIENTED_EDGE ( 'NONE', *, *, #9495, .F. ) ;
#2528 = DIRECTION ( 'NONE',  ( -1.820952055660014662E-28, -1.000000000000000000, 6.508102468073347395E-30 ) ) ;
#2529 = CARTESIAN_POINT ( 'NONE',  ( 5.775154784098243788, 58.97791112757358434, -35.56426808734907752 ) ) ;
#2530 = CARTESIAN_POINT ( 'NONE',  ( -7.848671329280705322, 59.99999999999999289, 32.05305536707737701 ) ) ;
#2531 = DIRECTION ( 'NONE',  ( -0.000000000000000000, -1.000000000000000000, -0.000000000000000000 ) ) ;
#2532 = LINE ( 'NONE', #5564, #1274 ) ;
#2533 = DIRECTION ( 'NONE',  ( 1.735493991486228775E-29, 0.000000000000000000, -1.000000000000000000 ) ) ;
#2534 = EDGE_CURVE ( 'NONE', #8621, #344, #4179, .T. ) ;
#2535 = VECTOR ( 'NONE', #5235, 1000.000000000000341 ) ;
#2536 = CARTESIAN_POINT ( 'NONE',  ( 28.37252191822215863, 30.00000000000000000, -6.000000000000006217 ) ) ;
#2537 = VERTEX_POINT ( 'NONE', #2839 ) ;
#2538 = CARTESIAN_POINT ( 'NONE',  ( -13.53485947486097984, 3.294852476641296768, 300.0000000000000000 ) ) ;
#2539 = DIRECTION ( 'NONE',  ( -0.9860132971832693549, -1.788557213313974126E-28, 0.1666666666666657970 ) ) ;
#2540 = ORIENTED_EDGE ( 'NONE', *, *, #169, .T. ) ;
#2541 = CARTESIAN_POINT ( 'NONE',  ( 9.082100980773736509, 61.99999999999999289, -35.86802812777734317 ) ) ;
#2542 = CARTESIAN_POINT ( 'NONE',  ( -8.545448575588386220, -1.757603667247791439E-27, -24.55555555555562108 ) ) ;
#2543 = ORIENTED_EDGE ( 'NONE', *, *, #1544, .F. ) ;
#2544 = CARTESIAN_POINT ( 'NONE',  ( -9.916130411093226016, 4.630053343978718594, 41.40967485888758404 ) ) ;
#2545 = VECTOR ( 'NONE', #6775, 1000.000000000000000 ) ;
#2546 = EDGE_CURVE ( 'NONE', #4052, #6324, #469, .T. ) ;
#2547 = PLANE ( 'NONE',  #4468 ) ;
#2548 = DIRECTION ( 'NONE',  ( 0.000000000000000000, 0.000000000000000000, 1.000000000000000000 ) ) ;
#2549 = EDGE_CURVE ( 'NONE', #6432, #279, #8686, .T. ) ;
#2550 = CARTESIAN_POINT ( 'NONE',  ( 6.030565054738658226, -4.722726170226616560, 38.63317537858744544 ) ) ;
#2551 = CIRCLE ( 'NONE', #1627, 5.000000000000000000 ) ;
#2552 = CARTESIAN_POINT ( 'NONE',  ( -24.67792535850613334, 28.99999999999997158, -3.999999999999997335 ) ) ;
#2553 = AXIS2_PLACEMENT_3D ( 'NONE', #4598, #740, #5334 ) ;
#2554 = ADVANCED_FACE ( 'NONE', ( #3444 ), #1957, .F. ) ;
#2555 = ORIENTED_EDGE ( 'NONE', *, *, #2746, .T. ) ;
#2556 = CARTESIAN_POINT ( 'NONE',  ( 32.21437568466744494, 59.99999999999997868, 7.920020133197005485 ) ) ;
#2557 = CARTESIAN_POINT ( 'NONE',  ( 0.000000000000000000, 59.99999999999999289, 0.000000000000000000 ) ) ;
#2558 = B_SPLINE_CURVE_WITH_KNOTS ( 'NONE', 3,
 ( #2541, #8495, #1862, #2492, #8535, #9284, #8584, #6256, #4881, #392 ),
 .UNSPECIFIED., .F., .F.,
 ( 4, 2, 2, 2, 4 ),
 ( 0.003057178249550609149, 0.004067793317122886214, 0.005078408384695163279, 0.006089023452267437742, 0.007099638519839713072 ),
 .UNSPECIFIED. ) ;
#2559 = ORIENTED_EDGE ( 'NONE', *, *, #3022, .F. ) ;
#2560 = ADVANCED_FACE ( 'NONE', ( #5715 ), #4978, .T. ) ;
#2561 = ADVANCED_FACE ( 'NONE', ( #9258 ), #5275, .F. ) ;
#2562 = EDGE_CURVE ( 'NONE', #5689, #1692, #2100, .T. ) ;
#2563 = CARTESIAN_POINT ( 'NONE',  ( 5.423418723394456162E-28, -2.066522830327504070E-28, -26.00000000000012790 ) ) ;
#2564 = CARTESIAN_POINT ( 'NONE',  ( 1.099474886651785204E-26, 54.50000000000031264, -37.00000000000000711 ) ) ;
#2565 = ORIENTED_EDGE ( 'NONE', *, *, #694, .F. ) ;
#2566 = DIRECTION ( 'NONE',  ( 0.000000000000000000, 1.000000000000000000, 0.000000000000000000 ) ) ;
#2567 = ORIENTED_EDGE ( 'NONE', *, *, #6152, .F. ) ;
#2568 = DIRECTION ( 'NONE',  ( 0.9444444444444403119, 0.000000000000000000, -0.3286710990611015903 ) ) ;
#2569 = VERTEX_POINT ( 'NONE', #95 ) ;
#2570 = ORIENTED_EDGE ( 'NONE', *, *, #3236, .T. ) ;
#2571 = CARTESIAN_POINT ( 'NONE',  ( -10.01570558914089126, -6.581988155506046212, 37.69304774390490564 ) ) ;
#2572 = DIRECTION ( 'NONE',  ( 0.000000000000000000, 1.000000000000000000, 0.000000000000000000 ) ) ;
#2573 = FACE_OUTER_BOUND ( 'NONE', #2163, .T. ) ;
#2574 = AXIS2_PLACEMENT_3D ( 'NONE', #8035, #2745, #3488 ) ;
#2575 = APPLICATION_CONTEXT ( 'automotive_design' ) ;
#2576 = PRODUCT_RELATED_PRODUCT_CATEGORY ( 'part', '', ( #786 ) ) ;
#2577 = ORIENTED_EDGE ( 'NONE', *, *, #4692, .F. ) ;
#2578 = ORIENTED_EDGE ( 'NONE', *, *, #1964, .T. ) ;
#2579 = DIRECTION ( 'NONE',  ( 0.000000000000000000, 0.000000000000000000, -1.000000000000000000 ) ) ;
#2580 = DIRECTION ( 'NONE',  ( -0.000000000000000000, 1.000000000000000000, -0.000000000000000000 ) ) ;
#2581 = CARTESIAN_POINT ( 'NONE',  ( 27.56211685706808723, 60.99999999999999289, 15.25056439471416780 ) ) ;
#2582 = AXIS2_PLACEMENT_3D ( 'NONE', #4626, #6968, #3774 ) ;
#2583 = CARTESIAN_POINT ( 'NONE',  ( 12.93945410785518924, -0.2138153430966752699, 36.79108894230666493 ) ) ;
#2584 = AXIS2_PLACEMENT_3D ( 'NONE', #6507, #455, #7302 ) ;
#2585 = FACE_OUTER_BOUND ( 'NONE', #81, .T. ) ;
#2586 = FACE_OUTER_BOUND ( 'NONE', #3346, .T. ) ;
#2587 = VECTOR ( 'NONE', #3203, 1000.000000000000000 ) ;
#2588 = AXIS2_PLACEMENT_3D ( 'NONE', #1268, #5711, #6396 ) ;
#2589 = DIRECTION ( 'NONE',  ( -0.000000000000000000, -1.000000000000000000, -0.000000000000000000 ) ) ;
#2590 = ORIENTED_EDGE ( 'NONE', *, *, #4639, .F. ) ;
#2591 = CARTESIAN_POINT ( 'NONE',  ( 33.06426808735054124, 61.99999999999999289, 5.562309845534586294 ) ) ;
#2592 = DIRECTION ( 'NONE',  ( 0.000000000000000000, 0.000000000000000000, 1.000000000000000000 ) ) ;
#2593 = PRODUCT ( 'Hardened Alloy Threading Chaser Dies', 'Hardened Alloy Threading Chaser Dies', '', ( #2958 ) ) ;
#2594 = AXIS2_PLACEMENT_3D ( 'NONE', #8798, #4454, #2019 ) ;
#2595 = ORIENTED_EDGE ( 'NONE', *, *, #4308, .T. ) ;
#2596 = DIRECTION ( 'NONE',  ( 0.000000000000000000, -1.000000000000000000, 0.000000000000000000 ) ) ;
#2597 = CARTESIAN_POINT ( 'NONE',  ( -6.000000000000005329, -15.00000000000000000, -31.00000000000000711 ) ) ;
#2598 = CIRCLE ( 'NONE', #2762, 37.00000000000000711 ) ;
#2599 = ORIENTED_EDGE ( 'NONE', *, *, #2844, .F. ) ;
#2600 = CARTESIAN_POINT ( 'NONE',  ( -13.23256407018424063, 1.700849823644902115, 36.68651977394890196 ) ) ;
#2601 = EDGE_CURVE ( 'NONE', #4748, #341, #8273, .T. ) ;
#2602 = FACE_OUTER_BOUND ( 'NONE', #8937, .T. ) ;
#2603 = CARTESIAN_POINT ( 'NONE',  ( 9.318419442923201951E-27, 44.00000000000019895, -25.00000000000000000 ) ) ;
#2604 = CIRCLE ( 'NONE', #3077, 34.50000000000000000 ) ;
#2605 = VECTOR ( 'NONE', #2360, 1000.000000000000000 ) ;
#2606 = DIRECTION ( 'NONE',  ( 0.000000000000000000, 0.000000000000000000, 1.000000000000000000 ) ) ;
#2607 = LINE ( 'NONE', #7103, #2285 ) ;
#2608 = ORIENTED_EDGE ( 'NONE', *, *, #7889, .T. ) ;
#2609 = CARTESIAN_POINT ( 'NONE',  ( 32.71871059427212458, 59.95478203631535052, 8.044358145045418240 ) ) ;
#2610 = EDGE_LOOP ( 'NONE', ( #9034, #3632, #8949, #660 ) ) ;
#2611 = DIRECTION ( 'NONE',  ( 0.000000000000000000, 1.000000000000000000, 0.000000000000000000 ) ) ;
#2612 = ORIENTED_EDGE ( 'NONE', *, *, #6627, .F. ) ;
#2613 = VECTOR ( 'NONE', #3594, 1000.000000000000000 ) ;
#2614 = CARTESIAN_POINT ( 'NONE',  ( -8.545448575588386220, 46.00000000000018474, -24.55555555555567793 ) ) ;
#2615 = CARTESIAN_POINT ( 'NONE',  ( -8.216777476527294510, 51.50000000000032685, -23.61111111111107519 ) ) ;
#2616 = UNCERTAINTY_MEASURE_WITH_UNIT (LENGTH_MEASURE( 1.000000000000000082E-05 ), #4951, 'distance_accuracy_value', 'NONE');
#2617 = EDGE_CURVE ( 'NONE', #7114, #5836, #4018, .T. ) ;
#2618 = VECTOR ( 'NONE', #1518, 1000.000000000000000 ) ;
#2619 = EDGE_CURVE ( 'NONE', #4852, #982, #8974, .T. ) ;
#2620 = CARTESIAN_POINT ( 'NONE',  ( 5.562309845534932684, 60.99999999999999289, -28.56426808735048439 ) ) ;
#2621 = ORIENTED_EDGE ( 'NONE', *, *, #3022, .T. ) ;
#2622 = DIRECTION ( 'NONE',  ( -0.000000000000000000, -1.000000000000000000, -0.000000000000000000 ) ) ;
#2623 = EDGE_CURVE ( 'NONE', #7113, #6031, #2183, .T. ) ;
#2624 = EDGE_LOOP ( 'NONE', ( #5586, #7289, #3456, #2219, #6564 ) ) ;
#2625 = CARTESIAN_POINT ( 'NONE',  ( -8.545448575588366680, 58.00000000000029132, -24.55555555555552161 ) ) ;
#2626 = ORIENTED_EDGE ( 'NONE', *, *, #4565, .F. ) ;
#2627 = ORIENTED_EDGE ( 'NONE', *, *, #7508, .F. ) ;
#2628 = CARTESIAN_POINT ( 'NONE',  ( -12.85843207060513116, 7.233932487497670927, 36.81975545894231061 ) ) ;
#2629 = DIRECTION ( 'NONE',  ( 0.000000000000000000, 0.000000000000000000, 1.000000000000000000 ) ) ;
#2630 = CARTESIAN_POINT ( 'NONE',  ( 2.200000000000000622, 0.000000000000000000, 2.199999999999999734 ) ) ;
#2631 = ORIENTED_EDGE ( 'NONE', *, *, #6119, .F. ) ;
#2632 = DIRECTION ( 'NONE',  ( -1.000000000000000000, -0.000000000000000000, -0.000000000000000000 ) ) ;
#2633 = DIRECTION ( 'NONE',  ( -0.9444444444444441977, 0.000000000000000000, 0.3286710990610907657 ) ) ;
#2634 = DIRECTION ( 'NONE',  ( 1.820952055660014662E-28, 1.000000000000000000, -6.508102468073347395E-30 ) ) ;
#2635 = DIRECTION ( 'NONE',  ( -0.9860132971832693549, -1.788557213313974126E-28, 0.1666666666666657970 ) ) ;
#2636 = PLANE ( 'NONE',  #2823 ) ;
#2637 = PLANE ( 'NONE',  #7435 ) ;
#2638 = CARTESIAN_POINT ( 'NONE',  ( 4.000000000000007994, 28.99999999999997158, 24.67792535850613334 ) ) ;
#2639 = CARTESIAN_POINT ( 'NONE',  ( 0.000000000000000000, 0.7216878364870328300, 1.250000000000000000 ) ) ;
#2640 = ORIENTED_EDGE ( 'NONE', *, *, #5180, .T. ) ;
#2641 = CARTESIAN_POINT ( 'NONE',  ( 0.01843853345419280837, 13.29483547765106799, 43.99999130734108377 ) ) ;
#2642 = ORIENTED_EDGE ( 'NONE', *, *, #5030, .F. ) ;
#2643 = CARTESIAN_POINT ( 'NONE',  ( 0.000000000000000000, 19.99999999999982236, -39.00000000000002132 ) ) ;
#2644 = CARTESIAN_POINT ( 'NONE',  ( 2.200000000000000178, 0.000000000000000000, 3.799999999999999378 ) ) ;
#2645 = VERTEX_POINT ( 'NONE', #3032 ) ;
#2646 = EDGE_CURVE ( 'NONE', #3069, #6892, #8333, .T. ) ;
#2647 = LINE ( 'NONE', #7295, #5444 ) ;
#2648 = DIRECTION ( 'NONE',  ( 1.000000000000000000, 0.000000000000000000, -2.168404344971006649E-16 ) ) ;
#2649 = CARTESIAN_POINT ( 'NONE',  ( -37.38678512219217254, 61.82631808411006347, -6.843790051325325585 ) ) ;
#2650 = ORIENTED_EDGE ( 'NONE', *, *, #8232, .T. ) ;
#2651 = DIRECTION ( 'NONE',  ( -0.3271946967961530950, 0.000000000000000000, 0.9449569463147374782 ) ) ;
#2652 = VERTEX_POINT ( 'NONE', #7548 ) ;
#2653 = CARTESIAN_POINT ( 'NONE',  ( -23.54759692749571087, 59.99999999999999289, 18.58791755254458522 ) ) ;
#2654 = DIRECTION ( 'NONE',  ( 0.000000000000000000, 0.000000000000000000, 1.000000000000000000 ) ) ;
#2655 = EDGE_LOOP ( 'NONE', ( #7603, #2961, #1699, #297 ) ) ;
#2656 = CYLINDRICAL_SURFACE ( 'NONE', #6642, 2.500000000000002220 ) ;
#2657 = AXIS2_PLACEMENT_3D ( 'NONE', #8324, #5893, #9653 ) ;
#2658 = DIRECTION ( 'NONE',  ( 0.000000000000000000, 0.000000000000000000, 1.000000000000000000 ) ) ;
#2659 = CARTESIAN_POINT ( 'NONE',  ( 0.01843853345419369655, 13.29483547765106977, 43.99999130734107666 ) ) ;
#2660 =( NAMED_UNIT ( * ) SI_UNIT ( $, .STERADIAN. ) SOLID_ANGLE_UNIT ( ) );
#2661 = ADVANCED_FACE ( 'NONE', ( #5176 ), #1198, .T. ) ;
#2662 = DIRECTION ( 'NONE',  ( 0.000000000000000000, 1.000000000000000000, 0.000000000000000000 ) ) ;
#2663 = ORIENTED_EDGE ( 'NONE', *, *, #2317, .F. ) ;
#2664 = DIRECTION ( 'NONE',  ( 0.000000000000000000, 0.000000000000000000, 1.000000000000000000 ) ) ;
#2665 = ORIENTED_EDGE ( 'NONE', *, *, #2977, .T. ) ;
#2666 = CARTESIAN_POINT ( 'NONE',  ( -29.00000000000000355, 30.00000000000000000, 0.000000000000000000 ) ) ;
#2667 = AXIS2_PLACEMENT_3D ( 'NONE', #8873, #5121, #2044 ) ;
#2668 = ORIENTED_EDGE ( 'NONE', *, *, #5762, .T. ) ;
#2669 = CARTESIAN_POINT ( 'NONE',  ( -7.944109461005667505, -2.787611319100306240, 42.35690170190217430 ) ) ;
#2670 = EDGE_CURVE ( 'NONE', #4372, #4366, #4200, .T. ) ;
#2671 = CARTESIAN_POINT ( 'NONE',  ( 4.904043666719842598, 60.99999999999999289, 31.11591804390326743 ) ) ;
#2672 = EDGE_CURVE ( 'NONE', #3565, #8321, #3071, .T. ) ;
#2673 = DIRECTION ( 'NONE',  ( 0.000000000000000000, 1.000000000000000000, 0.000000000000000000 ) ) ;
#2674 = EDGE_CURVE ( 'NONE', #6976, #2267, #1565, .T. ) ;
#2675 = CIRCLE ( 'NONE', #5532, 31.50000000000000000 ) ;
#2676 = ORIENTED_EDGE ( 'NONE', *, *, #4215, .F. ) ;
#2677 = CARTESIAN_POINT ( 'NONE',  ( 3.885274725274726393, -8.673617379884035472E-16, 0.000000000000000000 ) ) ;
#2678 = PLANE ( 'NONE',  #2738 ) ;
#2679 = EDGE_LOOP ( 'NONE', ( #1600, #9660, #8202, #5625, #143 ) ) ;
#2680 = DIRECTION ( 'NONE',  ( 0.6195972517514870548, -0.000000000000000000, 0.7849198975831892522 ) ) ;
#2681 = CARTESIAN_POINT ( 'NONE',  ( 1.820000000000000062, 0.000000000000000000, 0.000000000000000000 ) ) ;
#2682 = CARTESIAN_POINT ( 'NONE',  ( 9.762153702110021092E-27, 53.00000000000031974, -24.09806918451527835 ) ) ;
#2683 = CARTESIAN_POINT ( 'NONE',  ( -33.06426808735054124, 59.99999999999999289, -3.062309845534580077 ) ) ;
#2684 = AXIS2_PLACEMENT_3D ( 'NONE', #6033, #1605, #7683 ) ;
#2685 = EDGE_CURVE ( 'NONE', #9391, #7720, #7395, .T. ) ;
#2686 = DIRECTION ( 'NONE',  ( -0.9860132971832694659, -1.788557213313974350E-28, 0.1666666666666658247 ) ) ;
#2687 = EDGE_CURVE ( 'NONE', #4799, #49, #104, .T. ) ;
#2688 = EDGE_CURVE ( 'NONE', #1639, #7141, #7341, .T. ) ;
#2689 = B_SPLINE_CURVE_WITH_KNOTS ( 'NONE', 3,
 ( #5810, #5989, #6589, #6632 ),
 .UNSPECIFIED., .F., .F.,
 ( 4, 4 ),
 ( 0.000000000000000000, 0.001643226871903046308 ),
 .UNSPECIFIED. ) ;
#2690 = ORIENTED_EDGE ( 'NONE', *, *, #7129, .T. ) ;
#2691 = LINE ( 'NONE', #2094, #6253 ) ;
#2692 = DIRECTION ( 'NONE',  ( 0.000000000000000000, 0.000000000000000000, -1.000000000000000000 ) ) ;
#2693 = ORIENTED_EDGE ( 'NONE', *, *, #3729, .F. ) ;
#2694 = CARTESIAN_POINT ( 'NONE',  ( 33.06426808735054124, 61.99999999999999289, 5.562309845534586294 ) ) ;
#2695 =( NAMED_UNIT ( * ) SI_UNIT ( $, .STERADIAN. ) SOLID_ANGLE_UNIT ( ) );
#2696 = CARTESIAN_POINT ( 'NONE',  ( 0.000000000000000000, 30.00000000000000000, 0.000000000000000000 ) ) ;
#2697 = CARTESIAN_POINT ( 'NONE',  ( 0.000000000000000000, 59.99999999999999289, 0.000000000000000000 ) ) ;
#2698 = DIRECTION ( 'NONE',  ( -0.000000000000000000, -1.000000000000000000, -0.000000000000000000 ) ) ;
#2699 = CIRCLE ( 'NONE', #4140, 1.499999999999999556 ) ;
#2700 = ORIENTED_EDGE ( 'NONE', *, *, #3775, .T. ) ;
#2701 = LINE ( 'NONE', #3599, #5449 ) ;
#2702 = ADVANCED_FACE ( 'NONE', ( #2147 ), #8184, .F. ) ;
#2703 = ORIENTED_EDGE ( 'NONE', *, *, #9215, .T. ) ;
#2704 = CARTESIAN_POINT ( 'NONE',  ( 0.01225733702461903260, 18.29484822699931001, 38.99999871588790512 ) ) ;
#2705 = CARTESIAN_POINT ( 'NONE',  ( -10.07733521876669336, -14.99999999999807621, 37.15918820280854362 ) ) ;
#2706 = VECTOR ( 'NONE', #5501, 1000.000000000000000 ) ;
#2707 = ORIENTED_EDGE ( 'NONE', *, *, #1073, .T. ) ;
#2708 = DIRECTION ( 'NONE',  ( -1.000000000000000000, 0.000000000000000000, 0.000000000000000000 ) ) ;
#2709 = DIRECTION ( 'NONE',  ( -0.000000000000000000, -1.000000000000000000, -0.000000000000000000 ) ) ;
#2710 = VECTOR ( 'NONE', #5961, 1000.000000000000341 ) ;
#2711 = CONICAL_SURFACE ( 'NONE', #7777, 39.00000000000002132, 0.7853981633974431720 ) ;
#2712 = CARTESIAN_POINT ( 'NONE',  ( 3.604595221023451312, 12.64709689291967187, 38.88259557046998083 ) ) ;
#2713 = DIRECTION ( 'NONE',  ( 1.000000000000000000, -1.582067810090848070E-15, 1.049160758270772931E-14 ) ) ;
#2714 = VERTEX_POINT ( 'NONE', #9077 ) ;
#2715 = CARTESIAN_POINT ( 'NONE',  ( -33.06426808735054124, 59.99999999999999289, -5.562309845534581854 ) ) ;
#2716 = VERTEX_POINT ( 'NONE', #7442 ) ;
#2717 = CARTESIAN_POINT ( 'NONE',  ( 35.29563341415538247, 59.05475394944627965, 6.702038549863912564 ) ) ;
#2718 = ORIENTED_EDGE ( 'NONE', *, *, #9262, .T. ) ;
#2719 = VERTEX_POINT ( 'NONE', #1412 ) ;
#2720 = CARTESIAN_POINT ( 'NONE',  ( 0.02451486836953505749, 18.29482697815588921, 38.99999229514322252 ) ) ;
#2721 = VECTOR ( 'NONE', #4719, 1000.000000000000000 ) ;
#2722 = DIRECTION ( 'NONE',  ( 1.776356839400250465E-15, 0.000000000000000000, -1.000000000000000000 ) ) ;
#2723 = EDGE_CURVE ( 'NONE', #9614, #3486, #2293, .T. ) ;
#2724 = CARTESIAN_POINT ( 'NONE',  ( 11.80999999999999872, 0.000000000000000000, 0.000000000000000000 ) ) ;
#2725 = AXIS2_PLACEMENT_3D ( 'NONE', #3625, #7877, #3686 ) ;
#2726 = ORIENTED_EDGE ( 'NONE', *, *, #4275, .T. ) ;
#2727 = DIRECTION ( 'NONE',  ( -0.000000000000000000, -1.000000000000000000, -0.000000000000000000 ) ) ;
#2728 = EDGE_CURVE ( 'NONE', #3754, #2789, #7663, .T. ) ;
#2729 = DIRECTION ( 'NONE',  ( 1.000000000000000000, 0.000000000000000000, -1.084202172485503448E-16 ) ) ;
#2730 = ORIENTED_EDGE ( 'NONE', *, *, #6913, .T. ) ;
#2731 = VERTEX_POINT ( 'NONE', #7220 ) ;
#2732 = CARTESIAN_POINT ( 'NONE',  ( 0.000000000000000000, 28.99999999999997158, -29.00000000000000355 ) ) ;
#2733 = ADVANCED_FACE ( 'NONE', ( #5596 ), #9454, .T. ) ;
#2734 = CARTESIAN_POINT ( 'NONE',  ( 1.555535097482682654E-26, 78.08723716182652197, -25.00000000000000000 ) ) ;
#2735 = DIRECTION ( 'NONE',  ( -1.820952055660014662E-28, -1.000000000000000000, -7.038118388768679669E-30 ) ) ;
#2736 = DIRECTION ( 'NONE',  ( 0.000000000000000000, 0.000000000000000000, 1.000000000000000000 ) ) ;
#2737 = DIRECTION ( 'NONE',  ( 0.000000000000000000, 0.000000000000000000, -1.000000000000000000 ) ) ;
#2738 = AXIS2_PLACEMENT_3D ( 'NONE', #529, #6672, #8121 ) ;
#2739 = ADVANCED_FACE ( 'NONE', ( #8710 ), #7016, .F. ) ;
#2740 = VECTOR ( 'NONE', #712, 1000.000000000000000 ) ;
#2741 = ADVANCED_FACE ( 'NONE', ( #3369 ), #4023, .F. ) ;
#2742 = EDGE_LOOP ( 'NONE', ( #5941, #5386, #3180 ) ) ;
#2743 = AXIS2_PLACEMENT_3D ( 'NONE', #9717, #5127, #1514 ) ;
#2744 = DIRECTION ( 'NONE',  ( 0.000000000000000000, 0.000000000000000000, 1.000000000000000000 ) ) ;
#2745 = DIRECTION ( 'NONE',  ( 0.000000000000000000, 1.000000000000000000, 0.000000000000000000 ) ) ;
#2746 = EDGE_CURVE ( 'NONE', #8510, #3565, #8563, .T. ) ;
#2747 = ORIENTED_EDGE ( 'NONE', *, *, #4451, .F. ) ;
#2748 = CARTESIAN_POINT ( 'NONE',  ( 0.000000000000000000, 30.00000000000000000, 0.000000000000000000 ) ) ;
#2749 =( LENGTH_UNIT ( ) NAMED_UNIT ( * ) SI_UNIT ( .MILLI., .METRE. ) );
#2750 = PLANE ( 'NONE',  #8590 ) ;
#2751 = CARTESIAN_POINT ( 'NONE',  ( 10.23650415797109758, -5.544651734979271218, 37.65358413834264439 ) ) ;
#2752 = CIRCLE ( 'NONE', #5454, 1.500000000000001332 ) ;
#2753 = CARTESIAN_POINT ( 'NONE',  ( 2.200000000000000622, 0.000000000000000000, 0.000000000000000000 ) ) ;
#2754 = AXIS2_PLACEMENT_3D ( 'NONE', #1830, #3256, #355 ) ;
#2755 = CIRCLE ( 'NONE', #3242, 2.500000000000002220 ) ;
#2756 = ORIENTED_EDGE ( 'NONE', *, *, #3040, .F. ) ;
#2757 = DIRECTION ( 'NONE',  ( -1.084202172485503325E-16, 0.000000000000000000, -1.000000000000000000 ) ) ;
#2758 = CARTESIAN_POINT ( 'NONE',  ( 0.08302437902281271931, -15.00000000000000000, 30.58222658736175248 ) ) ;
#2759 = ORIENTED_EDGE ( 'NONE', *, *, #2130, .F. ) ;
#2760 = CARTESIAN_POINT ( 'NONE',  ( 0.000000000000000000, 54.99999999999999289, 0.000000000000000000 ) ) ;
#2761 = VECTOR ( 'NONE', #1383, 1000.000000000000000 ) ;
#2762 = AXIS2_PLACEMENT_3D ( 'NONE', #3215, #3317, #957 ) ;
#2763 = FACE_OUTER_BOUND ( 'NONE', #5287, .T. ) ;
#2764 = VECTOR ( 'NONE', #6634, 1000.000000000000000 ) ;
#2765 = AXIS2_PLACEMENT_3D ( 'NONE', #6760, #3208, #1693 ) ;
#2766 = CARTESIAN_POINT ( 'NONE',  ( 4.330416360834490774, 17.51076624374514523, 38.76727366216590553 ) ) ;
#2767 = CARTESIAN_POINT ( 'NONE',  ( 0.000000000000000000, 0.000000000000000000, 0.000000000000000000 ) ) ;
#2768 = FACE_OUTER_BOUND ( 'NONE', #1470, .T. ) ;
#2769 = ORIENTED_EDGE ( 'NONE', *, *, #7915, .T. ) ;
#2770 = FACE_OUTER_BOUND ( 'NONE', #4251, .T. ) ;
#2771 = PRODUCT_DEFINITION_CONTEXT ( 'detailed design', #2575, 'design' ) ;
#2772 = AXIS2_PLACEMENT_3D ( 'NONE', #7906, #1824, #6410 ) ;
#2773 = LINE ( 'NONE', #5792, #6923 ) ;
#2774 = DIRECTION ( 'NONE',  ( -0.000000000000000000, -1.000000000000000000, -0.000000000000000000 ) ) ;
#2775 = ORIENTED_EDGE ( 'NONE', *, *, #4415, .T. ) ;
#2776 = ORIENTED_EDGE ( 'NONE', *, *, #8975, .T. ) ;
#2777 = CARTESIAN_POINT ( 'NONE',  ( -0.3099780140802378403, 13.29544103063097893, 44.00030096464039531 ) ) ;
#2778 = CYLINDRICAL_SURFACE ( 'NONE', #727, 2.500000000000001332 ) ;
#2779 = LINE ( 'NONE', #8809, #998 ) ;
#2780 = ORIENTED_EDGE ( 'NONE', *, *, #6900, .F. ) ;
#2781 = LINE ( 'NONE', #5801, #8763 ) ;
#2782 = ORIENTED_EDGE ( 'NONE', *, *, #9508, .F. ) ;
#2783 = DIRECTION ( 'NONE',  ( 0.000000000000000000, 1.000000000000000000, 0.000000000000000000 ) ) ;
#2784 = DIRECTION ( 'NONE',  ( 0.000000000000000000, 0.000000000000000000, 1.000000000000000000 ) ) ;
#2785 = DIRECTION ( 'NONE',  ( -1.000000000000000000, 0.000000000000000000, 0.000000000000000000 ) ) ;
#2786 = LINE ( 'NONE', #5068, #5380 ) ;
#2787 = DIRECTION ( 'NONE',  ( 8.659560562354904508E-17, -0.7071067811865500152, 0.7071067811865451302 ) ) ;
#2788 = CARTESIAN_POINT ( 'NONE',  ( 0.000000000000000000, 1.443375672974065216, 1.084202172492522584E-16 ) ) ;
#2789 = VERTEX_POINT ( 'NONE', #8618 ) ;
#2790 = DIRECTION ( 'NONE',  ( 0.000000000000000000, 1.000000000000000000, 0.000000000000000000 ) ) ;
#2791 = CARTESIAN_POINT ( 'NONE',  ( 9.099351244776508807, 7.455330879947340783, 41.82994277301750685 ) ) ;
#2792 = VERTEX_POINT ( 'NONE', #9350 ) ;
#2793 = CARTESIAN_POINT ( 'NONE',  ( 35.88888888888889284, 39.99999999999999289, -12.48950176432140502 ) ) ;
#2794 = FACE_OUTER_BOUND ( 'NONE', #6929, .T. ) ;
#2795 = CARTESIAN_POINT ( 'NONE',  ( -12.78952641536645984, -0.8552499793260514016, 36.84380182560760630 ) ) ;
#2796 = EDGE_CURVE ( 'NONE', #2792, #7616, #6858, .T. ) ;
#2797 = ADVANCED_FACE ( 'NONE', ( #1843 ), #4859, .F. ) ;
#2798 = CARTESIAN_POINT ( 'NONE',  ( -5.000000000000006217, 30.00000000000000000, 0.000000000000000000 ) ) ;
#2799 = ADVANCED_FACE ( 'NONE', ( #7875 ), #6377, .F. ) ;
#2800 = DIRECTION ( 'NONE',  ( 0.000000000000000000, 0.000000000000000000, 1.000000000000000000 ) ) ;
#2801 = ORIENTED_EDGE ( 'NONE', *, *, #6425, .T. ) ;
#2802 = DIRECTION ( 'NONE',  ( 0.000000000000000000, 0.000000000000000000, 1.000000000000000000 ) ) ;
#2803 = CARTESIAN_POINT ( 'NONE',  ( -6.941591473825946323, -15.00000000000000178, 36.84329602096714495 ) ) ;
#2804 = EDGE_LOOP ( 'NONE', ( #9256, #826, #6072, #4131 ) ) ;
#2805 = EDGE_CURVE ( 'NONE', #4022, #2912, #7922, .T. ) ;
#2806 = FACE_OUTER_BOUND ( 'NONE', #7419, .T. ) ;
#2807 = DIRECTION ( 'NONE',  ( -0.000000000000000000, 1.000000000000000000, -0.000000000000000000 ) ) ;
#2808 = EDGE_CURVE ( 'NONE', #9409, #7344, #9396, .T. ) ;
#2809 = CARTESIAN_POINT ( 'NONE',  ( 3.257065296989332559, 12.77212832130460640, 43.73743695198545112 ) ) ;
#2810 = DIRECTION ( 'NONE',  ( 0.000000000000000000, 0.000000000000000000, 1.000000000000000000 ) ) ;
#2811 = ORIENTED_EDGE ( 'NONE', *, *, #1877, .T. ) ;
#2812 = DIRECTION ( 'NONE',  ( 0.000000000000000000, 1.000000000000000000, 0.000000000000000000 ) ) ;
#2813 = AXIS2_PLACEMENT_3D ( 'NONE', #1995, #2783, #4281 ) ;
#2814 = ORIENTED_EDGE ( 'NONE', *, *, #2977, .F. ) ;
#2815 = CARTESIAN_POINT ( 'NONE',  ( 35.42756555166880617, 59.00049740791308039, 6.394654627632705868 ) ) ;
#2816 = ORIENTED_EDGE ( 'NONE', *, *, #9461, .T. ) ;
#2817 = DIRECTION ( 'NONE',  ( -0.000000000000000000, -1.000000000000000000, -0.000000000000000000 ) ) ;
#2818 = VERTEX_POINT ( 'NONE', #9302 ) ;
#2819 = CARTESIAN_POINT ( 'NONE',  ( -4.407734956671747639, 12.30199650488687624, 38.81748064356022354 ) ) ;
#2820 = DIRECTION ( 'NONE',  ( -0.000000000000000000, 1.000000000000000000, -0.000000000000000000 ) ) ;
#2821 = CARTESIAN_POINT ( 'NONE',  ( -8.216777476527294510, 57.50000000000029843, -23.61111111111111427 ) ) ;
#2822 = AXIS2_PLACEMENT_3D ( 'NONE', #7850, #8491, #199 ) ;
#2823 = AXIS2_PLACEMENT_3D ( 'NONE', #581, #9559, #1220 ) ;
#2824 = ORIENTED_EDGE ( 'NONE', *, *, #5393, .F. ) ;
#2825 = LINE ( 'NONE', #8120, #6231 ) ;
#2826 = ORIENTED_EDGE ( 'NONE', *, *, #4692, .T. ) ;
#2827 = CARTESIAN_POINT ( 'NONE',  ( 5.423418723394456162E-28, -2.066522830327504070E-28, -26.00000000000017408 ) ) ;
#2828 = EDGE_CURVE ( 'NONE', #4569, #2443, #4124, .T. ) ;
#2829 = CARTESIAN_POINT ( 'NONE',  ( 0.000000000000000000, 59.99999999999999289, 0.000000000000000000 ) ) ;
#2830 = DIRECTION ( 'NONE',  ( 0.000000000000000000, 0.000000000000000000, 1.000000000000000000 ) ) ;
#2831 = CYLINDRICAL_SURFACE ( 'NONE', #3963, 31.50000000000000000 ) ;
#2832 = EDGE_CURVE ( 'NONE', #8061, #7838, #6276, .T. ) ;
#2833 = CARTESIAN_POINT ( 'NONE',  ( 1.094544505994153880E-26, 57.50000000000029843, -24.09806918451523217 ) ) ;
#2834 = VECTOR ( 'NONE', #3680, 1000.000000000000000 ) ;
#2835 = CARTESIAN_POINT ( 'NONE',  ( 4.000000000000001776, 28.99999999999997158, -24.67792535850613334 ) ) ;
#2836 = ORIENTED_EDGE ( 'NONE', *, *, #7330, .F. ) ;
#2837 = CARTESIAN_POINT ( 'NONE',  ( 0.000000000000000000, 60.99999999999999289, 0.000000000000000000 ) ) ;
#2838 = VECTOR ( 'NONE', #1024, 1000.000000000000000 ) ;
#2839 = CARTESIAN_POINT ( 'NONE',  ( -8.216777476527294510, 50.50000000000031974, -23.61111111111111427 ) ) ;
#2840 = ORIENTED_EDGE ( 'NONE', *, *, #521, .F. ) ;
#2841 = LINE ( 'NONE', #2643, #2878 ) ;
#2842 = DIRECTION ( 'NONE',  ( 1.000000000000000000, 0.000000000000000000, 0.000000000000000000 ) ) ;
#2843 =( GEOMETRIC_REPRESENTATION_CONTEXT ( 3 ) GLOBAL_UNCERTAINTY_ASSIGNED_CONTEXT ( ( #8322 ) ) GLOBAL_UNIT_ASSIGNED_CONTEXT ( ( #5849, #8867, #1501 ) ) REPRESENTATION_CONTEXT ( 'NONE', 'WORKASPACE' ) );
#2844 = EDGE_CURVE ( 'NONE', #5104, #1017, #7118, .T. ) ;
#2845 = CARTESIAN_POINT ( 'NONE',  ( 5.000000000000003553, 30.00000000000000000, -1.084202172485504040E-15 ) ) ;
#2846 = AXIS2_PLACEMENT_3D ( 'NONE', #5612, #1117, #1853 ) ;
#2847 = PRODUCT_DEFINITION_FORMATION_WITH_SPECIFIED_SOURCE ( 'ANY', '', #2593, .NOT_KNOWN. ) ;
#2848 = VERTEX_POINT ( 'NONE', #2625 ) ;
#2849 = LINE ( 'NONE', #8887, #5725 ) ;
#2850 = CARTESIAN_POINT ( 'NONE',  ( -6.850714362160835513, -15.00000000000000000, 28.25199985226410959 ) ) ;
#2851 = EDGE_CURVE ( 'NONE', #1692, #5689, #7181, .T. ) ;
#2852 = EDGE_LOOP ( 'NONE', ( #8155, #2377, #5734, #4966 ) ) ;
#2853 = AXIS2_PLACEMENT_3D ( 'NONE', #6562, #9585, #2802 ) ;
#2854 = CYLINDRICAL_SURFACE ( 'NONE', #1144, 38.00000000000000711 ) ;
#2855 = FACE_OUTER_BOUND ( 'NONE', #3763, .T. ) ;
#2856 = CARTESIAN_POINT ( 'NONE',  ( 0.000000000000000000, 60.99999999999999289, 0.000000000000000000 ) ) ;
#2857 = VERTEX_POINT ( 'NONE', #7825 ) ;
#2858 = CARTESIAN_POINT ( 'NONE',  ( 1.663275198395546939, 13.16107044704059881, 43.93189623020137446 ) ) ;
#2859 = CIRCLE ( 'NONE', #5712, 2.499999999999998668 ) ;
#2860 = ORIENTED_EDGE ( 'NONE', *, *, #6785, .T. ) ;
#2861 = DIRECTION ( 'NONE',  ( 0.000000000000000000, 0.000000000000000000, -1.000000000000000000 ) ) ;
#2862 = EDGE_CURVE ( 'NONE', #8986, #9386, #8944, .T. ) ;
#2863 = CARTESIAN_POINT ( 'NONE',  ( -3.999999999999999112, 28.99999999999997158, 24.67792535850613334 ) ) ;
#2864 = CARTESIAN_POINT ( 'NONE',  ( 1.084683744678891232E-26, 58.00000000000029132, -26.00000000000000355 ) ) ;
#2865 = EDGE_CURVE ( 'NONE', #1692, #5147, #7265, .T. ) ;
#2866 = ORIENTED_EDGE ( 'NONE', *, *, #3154, .T. ) ;
#2867 = LINE ( 'NONE', #1067, #2294 ) ;
#2868 = ORIENTED_EDGE ( 'NONE', *, *, #9331, .T. ) ;
#2869 = CARTESIAN_POINT ( 'NONE',  ( -6.030734287580929553, 11.33421872313606649, 38.63588227429310251 ) ) ;
#2870 = CARTESIAN_POINT ( 'NONE',  ( 0.000000000000000000, 61.99999999999999289, 0.000000000000000000 ) ) ;
#2871 = VECTOR ( 'NONE', #7541, 1000.000000000000000 ) ;
#2872 = DIRECTION ( 'NONE',  ( -0.7071067811865489050, 0.000000000000000000, 0.7071067811865462405 ) ) ;
#2873 = VERTEX_POINT ( 'NONE', #2864 ) ;
#2874 = DIRECTION ( 'NONE',  ( -1.820952055660014662E-28, -1.000000000000000000, -7.038118388768679669E-30 ) ) ;
#2875 = ORIENTED_EDGE ( 'NONE', *, *, #5710, .F. ) ;
#2876 = DIRECTION ( 'NONE',  ( 1.000000000000000000, -0.000000000000000000, 0.000000000000000000 ) ) ;
#2877 = TOROIDAL_SURFACE ( 'NONE', #5723, 29.00000000000001776, 10.00000000000000000 ) ;
#2878 = VECTOR ( 'NONE', #8878, 1000.000000000000000 ) ;
#2879 = DIRECTION ( 'NONE',  ( 0.000000000000000000, 0.000000000000000000, 1.000000000000000000 ) ) ;
#2880 =( NAMED_UNIT ( * ) SI_UNIT ( $, .STERADIAN. ) SOLID_ANGLE_UNIT ( ) );
#2881 = FACE_OUTER_BOUND ( 'NONE', #8106, .T. ) ;
#2882 = LINE ( 'NONE', #1364, #5603 ) ;
#2883 = CARTESIAN_POINT ( 'NONE',  ( 25.51470164434615029, 30.00000000000000000, 5.000000000000000888 ) ) ;
#2884 = DIRECTION ( 'NONE',  ( -0.000000000000000000, -1.000000000000000000, -0.000000000000000000 ) ) ;
#2885 = PLANE ( 'NONE',  #744 ) ;
#2886 = CARTESIAN_POINT ( 'NONE',  ( 0.000000000000000000, 58.99999999999999289, 0.000000000000000000 ) ) ;
#2887 = DIRECTION ( 'NONE',  ( -0.000000000000000000, 1.000000000000000000, -0.000000000000000000 ) ) ;
#2888 = DIRECTION ( 'NONE',  ( 1.820952055660014662E-28, 1.000000000000000000, 7.038118388768679669E-30 ) ) ;
#2889 = CARTESIAN_POINT ( 'NONE',  ( -1.288876940849657649, 18.24222776313161631, 38.98402153286875205 ) ) ;
#2890 = CIRCLE ( 'NONE', #7317, 4.500000000000004441 ) ;
#2891 = CARTESIAN_POINT ( 'NONE',  ( 31.00000000000000711, 27.42469319230601243, 6.000000000000000000 ) ) ;
#2892 = LINE ( 'NONE', #110, #1174 ) ;
#2893 = ORIENTED_EDGE ( 'NONE', *, *, #1774, .F. ) ;
#2894 = DIRECTION ( 'NONE',  ( 0.000000000000000000, 1.000000000000000000, 0.000000000000000000 ) ) ;
#2895 = CARTESIAN_POINT ( 'NONE',  ( 0.3577198796026725414, -15.00000000000000178, 30.56861933562558775 ) ) ;
#2896 = ORIENTED_EDGE ( 'NONE', *, *, #8248, .T. ) ;
#2897 = AXIS2_PLACEMENT_3D ( 'NONE', #3347, #1231, #496 ) ;
#2898 = CIRCLE ( 'NONE', #4187, 31.50000000000000000 ) ;
#2899 = CARTESIAN_POINT ( 'NONE',  ( 9.860761315262647568E-27, 51.50000000000032685, -26.00000000000008171 ) ) ;
#2900 = CARTESIAN_POINT ( 'NONE',  ( 26.32489316217636954, 30.00000000000000000, 6.000000000000000000 ) ) ;
#2901 = PLANE ( 'NONE',  #2349 ) ;
#2902 = ORIENTED_EDGE ( 'NONE', *, *, #9158, .T. ) ;
#2903 = CARTESIAN_POINT ( 'NONE',  ( 9.491487835072193846, 6.511041217878577037, 41.63483005588284414 ) ) ;
#2904 = CIRCLE ( 'NONE', #3706, 4.500000000000005329 ) ;
#2905 = SHAPE_DEFINITION_REPRESENTATION ( #6219, #551 ) ;
#2906 = VECTOR ( 'NONE', #7189, 1000.000000000000000 ) ;
#2907 = EDGE_LOOP ( 'NONE', ( #4763, #5693, #8433, #791 ) ) ;
#2908 = VERTEX_POINT ( 'NONE', #8161 ) ;
#2909 = CARTESIAN_POINT ( 'NONE',  ( -35.05384365671854852, 59.44855477671178079, -4.040090201280811755 ) ) ;
#2910 = ORIENTED_EDGE ( 'NONE', *, *, #9629, .T. ) ;
#2911 = CARTESIAN_POINT ( 'NONE',  ( 34.33638591132956464, 59.77059716828893698, 3.404146005973824440 ) ) ;
#2912 = VERTEX_POINT ( 'NONE', #5879 ) ;
#2913 = LINE ( 'NONE', #329, #4360 ) ;
#2914 = VERTEX_POINT ( 'NONE', #516 ) ;
#2915 = CIRCLE ( 'NONE', #9393, 26.00000000000012790 ) ;
#2916 = CARTESIAN_POINT ( 'NONE',  ( -7.285584084550976947, 10.15239125381765994, 42.62273125021567921 ) ) ;
#2917 = VECTOR ( 'NONE', #8352, 1000.000000000000000 ) ;
#2918 = VECTOR ( 'NONE', #8755, 1000.000000000000000 ) ;
#2919 = CARTESIAN_POINT ( 'NONE',  ( 1.040310318760209318E-26, 51.50000000000032685, -25.00000000000000000 ) ) ;
#2920 = CONICAL_SURFACE ( 'NONE', #4202, 39.00000000000002132, 0.7853981633974431720 ) ;
#2921 = CIRCLE ( 'NONE', #419, 18.51991245392837371 ) ;
#2922 = DIRECTION ( 'NONE',  ( 0.000000000000000000, 1.000000000000000000, 0.000000000000000000 ) ) ;
#2923 = EDGE_CURVE ( 'NONE', #8994, #5845, #8016, .T. ) ;
#2924 = EDGE_CURVE ( 'NONE', #2517, #1478, #7372, .T. ) ;
#2925 = EDGE_CURVE ( 'NONE', #77, #3257, #4312, .T. ) ;
#2926 = EDGE_CURVE ( 'NONE', #9428, #3135, #1497, .T. ) ;
#2927 = AXIS2_PLACEMENT_3D ( 'NONE', #6664, #9688, #3334 ) ;
#2928 = SHAPE_REPRESENTATION ( 'Covrt plate', ( #6314 ), #3968 ) ;
#2929 = CIRCLE ( 'NONE', #6867, 4.500000000000005329 ) ;
#2930 = EDGE_LOOP ( 'NONE', ( #2155, #2279, #2082, #5887 ) ) ;
#2931 = CARTESIAN_POINT ( 'NONE',  ( 0.000000000000000000, 38.99999999999993605, 0.000000000000000000 ) ) ;
#2932 = ORIENTED_EDGE ( 'NONE', *, *, #350, .F. ) ;
#2933 = PLANE ( 'NONE',  #3137 ) ;
#2934 = DIRECTION ( 'NONE',  ( 0.000000000000000000, 0.000000000000000000, 1.000000000000000000 ) ) ;
#2935 = SURFACE_STYLE_USAGE ( .BOTH. , #6676 ) ;
#2936 = VECTOR ( 'NONE', #8837, 1000.000000000000000 ) ;
#2937 = LINE ( 'NONE', #7391, #2507 ) ;
#2938 = ORIENTED_EDGE ( 'NONE', *, *, #7225, .F. ) ;
#2939 = DIRECTION ( 'NONE',  ( -6.982962677686269077E-15, 0.000000000000000000, 1.000000000000000000 ) ) ;
#2940 = DIRECTION ( 'NONE',  ( -0.000000000000000000, -1.000000000000000000, -0.000000000000000000 ) ) ;
#2941 = DIRECTION ( 'NONE',  ( 0.000000000000000000, 0.000000000000000000, 1.000000000000000000 ) ) ;
#2942 = CARTESIAN_POINT ( 'NONE',  ( 1.148778693228098442E-26, 59.00000000000029843, -26.00000000000000355 ) ) ;
#2943 = CIRCLE ( 'NONE', #8475, 17.99999999999999645 ) ;
#2944 = CARTESIAN_POINT ( 'NONE',  ( -5.012544999578074645, 17.20596322573581105, 38.68080642594335927 ) ) ;
#2945 = EDGE_CURVE ( 'NONE', #294, #3288, #7172, .T. ) ;
#2946 = ORIENTED_EDGE ( 'NONE', *, *, #5705, .T. ) ;
#2947 = DIRECTION ( 'NONE',  ( -1.820952055660014662E-28, -1.000000000000000000, -7.038118388768679669E-30 ) ) ;
#2948 = ADVANCED_FACE ( 'NONE', ( #5197 ), #5154, .T. ) ;
#2949 = VERTEX_POINT ( 'NONE', #4409 ) ;
#2950 = LINE ( 'NONE', #1579, #6192 ) ;
#2951 = CARTESIAN_POINT ( 'NONE',  ( 1.338007665914787259, -9.401856577713825658, 39.49693264723424591 ) ) ;
#2952 = ORIENTED_EDGE ( 'NONE', *, *, #4051, .T. ) ;
#2953 = DIRECTION ( 'NONE',  ( 0.000000000000000000, 0.000000000000000000, -1.000000000000000000 ) ) ;
#2954 = CARTESIAN_POINT ( 'NONE',  ( -26.32489316217636954, 30.00000000000000000, 6.000000000000009770 ) ) ;
#2955 = ORIENTED_EDGE ( 'NONE', *, *, #3964, .T. ) ;
#2956 = EDGE_CURVE ( 'NONE', #9742, #9391, #8804, .T. ) ;
#2957 = CARTESIAN_POINT ( 'NONE',  ( 7.517587493874460236, -3.331319210360449201, 42.53641844432376473 ) ) ;
#2958 = PRODUCT_CONTEXT ( 'NONE', #4296, 'mechanical' ) ;
#2959 = ORIENTED_EDGE ( 'NONE', *, *, #4249, .F. ) ;
#2960 = CARTESIAN_POINT ( 'NONE',  ( -25.51470164434615029, 30.00000000000000000, -4.999999999999997335 ) ) ;
#2961 = ORIENTED_EDGE ( 'NONE', *, *, #9244, .T. ) ;
#2962 = FACE_OUTER_BOUND ( 'NONE', #1781, .T. ) ;
#2963 = ORIENTED_EDGE ( 'NONE', *, *, #6261, .F. ) ;
#2964 = CARTESIAN_POINT ( 'NONE',  ( 5.562309845534588959, 49.99999999999999289, -33.06426808735054124 ) ) ;
#2965 = VERTEX_POINT ( 'NONE', #5050 ) ;
#2966 = CARTESIAN_POINT ( 'NONE',  ( -5.302731225069202026, 11.77929979337195654, 43.27702668925476104 ) ) ;
#2967 = DIRECTION ( 'NONE',  ( 0.000000000000000000, 0.000000000000000000, -1.000000000000000000 ) ) ;
#2968 = CARTESIAN_POINT ( 'NONE',  ( -29.00000000000000355, 28.99999999999997158, 4.000000000000010658 ) ) ;
#2969 = EDGE_CURVE ( 'NONE', #5003, #5845, #4665, .T. ) ;
#2970 = EDGE_CURVE ( 'NONE', #4052, #9341, #610, .T. ) ;
#2971 = ORIENTED_EDGE ( 'NONE', *, *, #5705, .F. ) ;
#2972 = DIRECTION ( 'NONE',  ( 0.000000000000000000, 0.000000000000000000, 1.000000000000000000 ) ) ;
#2973 = VERTEX_POINT ( 'NONE', #3612 ) ;
#2974 = ADVANCED_FACE ( 'NONE', ( #5446 ), #3760, .F. ) ;
#2975 = CARTESIAN_POINT ( 'NONE',  ( 6.000000000000001776, 30.00000000000000000, -28.37252191822216218 ) ) ;
#2976 = CARTESIAN_POINT ( 'NONE',  ( 0.000000000000000000, 0.000000000000000000, 0.000000000000000000 ) ) ;
#2977 = EDGE_CURVE ( 'NONE', #4609, #285, #3108, .T. ) ;
#2978 = CARTESIAN_POINT ( 'NONE',  ( 0.000000000000000000, 0.000000000000000000, 0.000000000000000000 ) ) ;
#2979 = CARTESIAN_POINT ( 'NONE',  ( -28.34870838944214455, 39.99999999999999289, -9.815840903884556212 ) ) ;
#2980 = AXIS2_PLACEMENT_3D ( 'NONE', #1125, #7288, #7138 ) ;
#2981 = CIRCLE ( 'NONE', #4577, 0.2000000000000000944 ) ;
#2982 = CARTESIAN_POINT ( 'NONE',  ( 4.665243217607700998, 29.66524321760768501, -25.23917843705063646 ) ) ;
#2983 = EDGE_CURVE ( 'NONE', #1828, #7231, #8405, .T. ) ;
#2984 = ORIENTED_EDGE ( 'NONE', *, *, #1550, .F. ) ;
#2985 = DIRECTION ( 'NONE',  ( 0.000000000000000000, 0.000000000000000000, 1.000000000000000000 ) ) ;
#2986 = CARTESIAN_POINT ( 'NONE',  ( -8.216777476527294510, 42.50000000000020606, -23.61111111111107519 ) ) ;
#2987 = EDGE_CURVE ( 'NONE', #5863, #9011, #127, .T. ) ;
#2988 = CARTESIAN_POINT ( 'NONE',  ( 6.000000000000001776, 27.42469319230600533, -31.00000000000000711 ) ) ;
#2989 = CIRCLE ( 'NONE', #3793, 2.000000000000000000 ) ;
#2990 = EDGE_CURVE ( 'NONE', #9346, #7747, #2207, .T. ) ;
#2991 = EDGE_CURVE ( 'NONE', #8562, #4542, #685, .T. ) ;
#2992 = AXIS2_PLACEMENT_3D ( 'NONE', #3134, #5376, #7694 ) ;
#2993 = CARTESIAN_POINT ( 'NONE',  ( 1.555535097482682654E-26, 78.08723716182652197, -25.00000000000000000 ) ) ;
#2994 = ORIENTED_EDGE ( 'NONE', *, *, #2486, .F. ) ;
#2995 = LINE ( 'NONE', #8239, #8390 ) ;
#2996 = CARTESIAN_POINT ( 'NONE',  ( 5.828629696051876863, -14.99999999999999822, 28.64426056422739464 ) ) ;
#2997 = EDGE_CURVE ( 'NONE', #6561, #915, #4035, .T. ) ;
#2998 = VERTEX_POINT ( 'NONE', #2363 ) ;
#2999 = DIRECTION ( 'NONE',  ( 0.000000000000000000, 1.000000000000000000, 0.000000000000000000 ) ) ;
#3000 = CARTESIAN_POINT ( 'NONE',  ( 3.153634179030674556, 61.99999999999999289, -36.86535760663186068 ) ) ;
#3001 = ADVANCED_FACE ( 'NONE', ( #2962 ), #2278, .F. ) ;
#3002 = CARTESIAN_POINT ( 'NONE',  ( 8.350939762285211287, -2.249335134881106590, 38.23794203041205719 ) ) ;
#3003 = CONTEXT_DEPENDENT_SHAPE_REPRESENTATION ( #6113, #8440 ) ;
#3004 = AXIS2_PLACEMENT_3D ( 'NONE', #7963, #9398, #9488 ) ;
#3005 = ORIENTED_EDGE ( 'NONE', *, *, #4933, .T. ) ;
#3006 = DIRECTION ( 'NONE',  ( 1.735493991486226532E-29, 0.000000000000000000, -1.000000000000000000 ) ) ;
#3007 = DIRECTION ( 'NONE',  ( -0.000000000000000000, -1.000000000000000000, -0.000000000000000000 ) ) ;
#3008 = CARTESIAN_POINT ( 'NONE',  ( 6.000000000000007994, 30.00000000000000000, 28.37252191822215863 ) ) ;
#3009 = ORIENTED_EDGE ( 'NONE', *, *, #5108, .T. ) ;
#3010 = DIRECTION ( 'NONE',  ( 1.735493991486225972E-29, -6.508102468073347395E-30, -1.000000000000000000 ) ) ;
#3011 = EDGE_LOOP ( 'NONE', ( #9123, #2321, #3611, #7563 ) ) ;
#3012 = CARTESIAN_POINT ( 'NONE',  ( -4.007938479032604917, 27.75794689997812270, -31.00000000000001066 ) ) ;
#3013 = CARTESIAN_POINT ( 'NONE',  ( 29.00000000000000355, 0.000000000000000000, -4.000000000000007105 ) ) ;
#3014 = CARTESIAN_POINT ( 'NONE',  ( -3.153634179030417872, 61.99999999999999289, 36.86535760663188199 ) ) ;
#3015 = VECTOR ( 'NONE', #1290, 1000.000000000000341 ) ;
#3016 = ORIENTED_EDGE ( 'NONE', *, *, #889, .T. ) ;
#3017 = CARTESIAN_POINT ( 'NONE',  ( -7.548108395552116434, 59.38382381638699314, 34.59619211116746129 ) ) ;
#3018 = ORIENTED_EDGE ( 'NONE', *, *, #5478, .T. ) ;
#3019 = VERTEX_POINT ( 'NONE', #8459 ) ;
#3020 = CARTESIAN_POINT ( 'NONE',  ( 0.000000000000000000, 38.99999999999993605, 17.99999999999999645 ) ) ;
#3021 = CYLINDRICAL_SURFACE ( 'NONE', #7482, 26.00000000000003197 ) ;
#3022 = EDGE_CURVE ( 'NONE', #2714, #1495, #7331, .T. ) ;
#3023 = VECTOR ( 'NONE', #7045, 1000.000000000000000 ) ;
#3024 = DIRECTION ( 'NONE',  ( -0.000000000000000000, 1.000000000000000000, -0.000000000000000000 ) ) ;
#3025 = CARTESIAN_POINT ( 'NONE',  ( -8.545448575588366680, -1.757025888264475269E-27, -24.55555555555556424 ) ) ;
#3026 = AXIS2_PLACEMENT_3D ( 'NONE', #221, #4562, #2370 ) ;
#3027 = VERTEX_POINT ( 'NONE', #3862 ) ;
#3028 = CYLINDRICAL_SURFACE ( 'NONE', #1111, 17.99999999999999645 ) ;
#3029 = VECTOR ( 'NONE', #7095, 1000.000000000000000 ) ;
#3030 = ORIENTED_EDGE ( 'NONE', *, *, #7565, .F. ) ;
#3031 = LINE ( 'NONE', #2986, #5852 ) ;
#3032 = CARTESIAN_POINT ( 'NONE',  ( -5.371095444502437921, 61.99999999999999289, -34.07933880998933773 ) ) ;
#3033 = CARTESIAN_POINT ( 'NONE',  ( 0.000000000000000000, -15.00000000000000000, 39.00000000000002132 ) ) ;
#3034 = CARTESIAN_POINT ( 'NONE',  ( 1.030449557444946671E-26, 48.50000000000033396, -25.00000000000000000 ) ) ;
#3035 = CARTESIAN_POINT ( 'NONE',  ( 0.000000000000000000, 0.000000000000000000, 0.000000000000000000 ) ) ;
#3036 = EDGE_LOOP ( 'NONE', ( #1378, #1929, #3940, #8036 ) ) ;
#3037 = LINE ( 'NONE', #5272, #715 ) ;
#3038 = EDGE_CURVE ( 'NONE', #5882, #9092, #906, .T. ) ;
#3039 = EDGE_CURVE ( 'NONE', #9639, #22, #9516, .T. ) ;
#3040 = EDGE_CURVE ( 'NONE', #7361, #3246, #8255, .T. ) ;
#3041 = CARTESIAN_POINT ( 'NONE',  ( 0.000000000000000000, 39.99999999999999289, 0.000000000000000000 ) ) ;
#3042 = ORIENTED_EDGE ( 'NONE', *, *, #7891, .T. ) ;
#3043 = DIRECTION ( 'NONE',  ( -0.000000000000000000, -1.000000000000000000, -0.000000000000000000 ) ) ;
#3044 = CARTESIAN_POINT ( 'NONE',  ( 1.072424122083380116, -9.427504479632391465, 39.50837534435000720 ) ) ;
#3045 = VERTEX_POINT ( 'NONE', #1482 ) ;
#3046 = LINE ( 'NONE', #5338, #3501 ) ;
#3047 = VECTOR ( 'NONE', #2539, 1000.000000000000341 ) ;
#3048 = CARTESIAN_POINT ( 'NONE',  ( 4.104483837744082209, 61.95009619975343185, -37.32687308866057663 ) ) ;
#3049 = ORIENTED_EDGE ( 'NONE', *, *, #1214, .F. ) ;
#3050 = EDGE_CURVE ( 'NONE', #7231, #2998, #6441, .T. ) ;
#3051 = CARTESIAN_POINT ( 'NONE',  ( 9.914908413137576204, 1.791417294963860041, 37.88076626776848599 ) ) ;
#3052 = VECTOR ( 'NONE', #3380, 1000.000000000000000 ) ;
#3053 = ORIENTED_EDGE ( 'NONE', *, *, #3736, .T. ) ;
#3054 = DIRECTION ( 'NONE',  ( 1.735493991486226532E-29, 0.000000000000000000, -1.000000000000000000 ) ) ;
#3055 = CIRCLE ( 'NONE', #5745, 1.000000000000000888 ) ;
#3056 = CARTESIAN_POINT ( 'NONE',  ( 25.23917843705063646, 29.66524321760768501, 4.665243217607698334 ) ) ;
#3057 = ORIENTED_EDGE ( 'NONE', *, *, #9280, .T. ) ;
#3058 = CARTESIAN_POINT ( 'NONE',  ( 1.030449557444946671E-26, 48.50000000000033396, -25.00000000000000000 ) ) ;
#3059 = CIRCLE ( 'NONE', #4340, 3.799999999999999378 ) ;
#3060 = ORIENTED_EDGE ( 'NONE', *, *, #8682, .T. ) ;
#3061 = CARTESIAN_POINT ( 'NONE',  ( 33.06426808735054124, 49.99999999999999289, 5.562309845534586294 ) ) ;
#3062 = PLANE ( 'NONE',  #2765 ) ;
#3063 = DIRECTION ( 'NONE',  ( -0.9860132971832693549, -1.788557213313974126E-28, 0.1666666666666657970 ) ) ;
#3064 = VECTOR ( 'NONE', #7910, 1000.000000000000000 ) ;
#3065 = AXIS2_PLACEMENT_3D ( 'NONE', #4972, #9318, #2533 ) ;
#3066 = ORIENTED_EDGE ( 'NONE', *, *, #6665, .F. ) ;
#3067 = CARTESIAN_POINT ( 'NONE',  ( -7.848671329280705322, 59.99999999999999289, 32.05305536707737701 ) ) ;
#3068 = AXIS2_PLACEMENT_3D ( 'NONE', #8399, #9192, #1584 ) ;
#3069 = VERTEX_POINT ( 'NONE', #7615 ) ;
#3070 = VECTOR ( 'NONE', #5407, 1000.000000000000000 ) ;
#3071 = CIRCLE ( 'NONE', #5609, 33.00000000000000000 ) ;
#3072 = EDGE_LOOP ( 'NONE', ( #6255, #4777, #5571, #1543 ) ) ;
#3073 = TOROIDAL_SURFACE ( 'NONE', #573, 33.00000000000000711, 5.000000000000000000 ) ;
#3074 = CARTESIAN_POINT ( 'NONE',  ( -4.738789600095485888, -10.72862449626830106, 38.71314812621989887 ) ) ;
#3075 = DIRECTION ( 'NONE',  ( 0.000000000000000000, -1.000000000000000000, 0.000000000000000000 ) ) ;
#3076 = FACE_OUTER_BOUND ( 'NONE', #8023, .T. ) ;
#3077 = AXIS2_PLACEMENT_3D ( 'NONE', #4002, #5492, #2496 ) ;
#3078 = CIRCLE ( 'NONE', #5618, 4.999999999999999112 ) ;
#3079 = ORIENTED_EDGE ( 'NONE', *, *, #3207, .F. ) ;
#3080 = CARTESIAN_POINT ( 'NONE',  ( 12.48950176432140680, 59.99999999999999289, 35.88888888888889284 ) ) ;
#3081 = DIRECTION ( 'NONE',  ( -0.000000000000000000, 0.000000000000000000, -1.000000000000000000 ) ) ;
#3082 = VERTEX_POINT ( 'NONE', #2263 ) ;
#3083 = CARTESIAN_POINT ( 'NONE',  ( 2.200000000000000178, 0.000000000000000000, 0.000000000000000000 ) ) ;
#3084 = CARTESIAN_POINT ( 'NONE',  ( 0.000000000000000000, 59.99999999999999289, 0.000000000000000000 ) ) ;
#3085 = DIRECTION ( 'NONE',  ( 0.000000000000000000, 1.000000000000000000, -0.000000000000000000 ) ) ;
#3086 = CARTESIAN_POINT ( 'NONE',  ( -7.537829016256761605, -15.00000000000000178, 28.01273236561391045 ) ) ;
#3087 = CARTESIAN_POINT ( 'NONE',  ( 9.860761315262647568E-27, 47.50000000000033396, -24.09806918451532809 ) ) ;
#3088 = CARTESIAN_POINT ( 'NONE',  ( 15.25056439471407188, 61.99999999999999289, -27.56211685706813341 ) ) ;
#3089 = APPLICATION_CONTEXT ( 'automotive_design' ) ;
#3090 = DIRECTION ( 'NONE',  ( -0.3286710990611143579, -1.387778780781445676E-15, -0.9444444444444359821 ) ) ;
#3091 = VECTOR ( 'NONE', #9294, 1000.000000000000341 ) ;
#3092 = DIRECTION ( 'NONE',  ( 0.000000000000000000, 0.000000000000000000, -1.000000000000000000 ) ) ;
#3093 = CARTESIAN_POINT ( 'NONE',  ( 0.000000000000000000, 59.99999999999999289, 0.000000000000000000 ) ) ;
#3094 = ORIENTED_EDGE ( 'NONE', *, *, #1386, .F. ) ;
#3095 = PLANE ( 'NONE',  #4635 ) ;
#3096 = CARTESIAN_POINT ( 'NONE',  ( 5.021056721195745531, -14.99999999999936229, 36.79118000870545302 ) ) ;
#3097 = EDGE_LOOP ( 'NONE', ( #8573, #8616, #5009, #2627 ) ) ;
#3098 = ADVANCED_FACE ( 'NONE', ( #6017 ), #3917, .T. ) ;
#3099 = ADVANCED_FACE ( 'NONE', ( #8354 ), #1592, .F. ) ;
#3100 = CARTESIAN_POINT ( 'NONE',  ( 18.51991245392837371, 3.294852476641296768, 294.6136752714472777 ) ) ;
#3101 = DIRECTION ( 'NONE',  ( 0.3286710990610922090, 6.289316826390952918E-29, 0.9444444444444435316 ) ) ;
#3102 = ORIENTED_EDGE ( 'NONE', *, *, #2191, .F. ) ;
#3103 = CARTESIAN_POINT ( 'NONE',  ( 11.27186822886705642, -4.675031839269720990, 37.33643085324619904 ) ) ;
#3104 = B_SPLINE_CURVE_WITH_KNOTS ( 'NONE', 3,
 ( #1417, #4437, #6640, #681, #6937, #4645, #5429, #4784 ),
 .UNSPECIFIED., .F., .F.,
 ( 4, 2, 2, 4 ),
 ( 8.673617379884035472E-19, 0.006005055813302546432, 0.009007583719953818346, 0.01201011162660509113 ),
 .UNSPECIFIED. ) ;
#3105 = ORIENTED_EDGE ( 'NONE', *, *, #8964, .F. ) ;
#3106 = CYLINDRICAL_SURFACE ( 'NONE', #7673, 1.500000000000000888 ) ;
#3107 = DIRECTION ( 'NONE',  ( -0.3286710990610922090, -6.289316826390952918E-29, -0.9444444444444435316 ) ) ;
#3108 = LINE ( 'NONE', #4509, #9237 ) ;
#3109 = ORIENTED_EDGE ( 'NONE', *, *, #6186, .T. ) ;
#3110 = DIRECTION ( 'NONE',  ( 0.5773502691896204020, -0.5773502691896366112, 0.5773502691896204020 ) ) ;
#3111 = EDGE_LOOP ( 'NONE', ( #4583, #7158, #2420, #5880, #3513, #1741, #7193, #6576 ) ) ;
#3112 = EDGE_CURVE ( 'NONE', #8252, #7059, #8916, .T. ) ;
#3113 = LINE ( 'NONE', #5401, #6214 ) ;
#3114 = EDGE_CURVE ( 'NONE', #6663, #3981, #8550, .T. ) ;
#3115 = CARTESIAN_POINT ( 'NONE',  ( 32.59762842694625817, 60.99999999999999289, -3.637569555611369854 ) ) ;
#3116 = CARTESIAN_POINT ( 'NONE',  ( -4.716066576642697683, 61.89689025924450760, 37.50432491070257868 ) ) ;
#3117 = ORIENTED_EDGE ( 'NONE', *, *, #7585, .F. ) ;
#3118 = DIRECTION ( 'NONE',  ( 0.000000000000000000, 1.000000000000000000, 0.000000000000000000 ) ) ;
#3119 = ORIENTED_EDGE ( 'NONE', *, *, #8557, .T. ) ;
#3120 = ORIENTED_EDGE ( 'NONE', *, *, #2184, .T. ) ;
#3121 = DIRECTION ( 'NONE',  ( 2.168404344971006649E-16, -0.000000000000000000, 1.000000000000000000 ) ) ;
#3122 =( LENGTH_UNIT ( ) NAMED_UNIT ( * ) SI_UNIT ( .MILLI., .METRE. ) );
#3123 = CARTESIAN_POINT ( 'NONE',  ( 11.07761026121386294, -5.000000000000018652, 37.39366993089406321 ) ) ;
#3124 = EDGE_CURVE ( 'NONE', #7306, #8835, #6688, .T. ) ;
#3125 = ORIENTED_EDGE ( 'NONE', *, *, #7989, .T. ) ;
#3126 = LINE ( 'NONE', #773, #1583 ) ;
#3127 = FACE_OUTER_BOUND ( 'NONE', #546, .T. ) ;
#3128 = CARTESIAN_POINT ( 'NONE',  ( -4.397412886516822716, 59.29888504437717955, 35.28275170782141146 ) ) ;
#3129 = ORIENTED_EDGE ( 'NONE', *, *, #7939, .F. ) ;
#3130 = LINE ( 'NONE', #9127, #2447 ) ;
#3131 = DIRECTION ( 'NONE',  ( 1.000000000000000000, 0.000000000000000000, 3.491481338843137300E-15 ) ) ;
#3132 = DIRECTION ( 'NONE',  ( -1.820952055660014662E-28, -1.000000000000000000, -7.038118388768679669E-30 ) ) ;
#3133 = FACE_OUTER_BOUND ( 'NONE', #7919, .T. ) ;
#3134 = CARTESIAN_POINT ( 'NONE',  ( 1.300000000000000044, -0.7216878364870317197, -1.250000000000000000 ) ) ;
#3135 = VERTEX_POINT ( 'NONE', #7155 ) ;
#3136 = DIRECTION ( 'NONE',  ( -1.820952055660014662E-28, -1.000000000000000000, -7.038118388768679669E-30 ) ) ;
#3137 = AXIS2_PLACEMENT_3D ( 'NONE', #5983, #2280, #6674 ) ;
#3138 = DIRECTION ( 'NONE',  ( -0.000000000000000000, -1.000000000000000000, -0.000000000000000000 ) ) ;
#3139 = CIRCLE ( 'NONE', #2980, 30.00000000000001066 ) ;
#3140 = TOROIDAL_SURFACE ( 'NONE', #5204, 13.53485947486097984, 5.000000000000000000 ) ;
#3141 = DIRECTION ( 'NONE',  ( -1.000000000000000000, 0.000000000000000000, -3.083952846180987322E-15 ) ) ;
#3142 = VERTEX_POINT ( 'NONE', #267 ) ;
#3143 = LINE ( 'NONE', #2352, #2227 ) ;
#3144 = CARTESIAN_POINT ( 'NONE',  ( 37.13646476935431195, 61.98650506287648909, 3.627735144839754344 ) ) ;
#3145 = ORIENTED_EDGE ( 'NONE', *, *, #4319, .F. ) ;
#3146 = EDGE_CURVE ( 'NONE', #5052, #1776, #5290, .T. ) ;
#3147 = DIRECTION ( 'NONE',  ( 0.000000000000000000, 0.000000000000000000, 1.000000000000000000 ) ) ;
#3148 = AXIS2_PLACEMENT_3D ( 'NONE', #8501, #1730, #4749 ) ;
#3149 = CARTESIAN_POINT ( 'NONE',  ( 24.67792535850613334, 28.99999999999997158, 4.000000000000000888 ) ) ;
#3150 = EDGE_LOOP ( 'NONE', ( #3322, #2775, #9592, #5647, #7325 ) ) ;
#3151 = CARTESIAN_POINT ( 'NONE',  ( 1.076825440025126701, -6.664617900633762027, 38.99321102797971861 ) ) ;
#3152 = CONTEXT_DEPENDENT_SHAPE_REPRESENTATION ( #7959, #873 ) ;
#3153 = CARTESIAN_POINT ( 'NONE',  ( -25.23917843705063646, 29.66524321760768501, -4.665243217607696558 ) ) ;
#3154 = EDGE_CURVE ( 'NONE', #427, #209, #7973, .T. ) ;
#3155 = VECTOR ( 'NONE', #7194, 1000.000000000000000 ) ;
#3156 = CARTESIAN_POINT ( 'NONE',  ( 0.000000000000000000, 30.00000000000000000, 0.000000000000000000 ) ) ;
#3157 = CARTESIAN_POINT ( 'NONE',  ( 6.000000000000007994, 27.42469319230600533, 31.00000000000000711 ) ) ;
#3158 = ORIENTED_EDGE ( 'NONE', *, *, #7254, .T. ) ;
#3159 = CARTESIAN_POINT ( 'NONE',  ( -30.18708036726492594, 60.99999999999999289, -16.70299909897287094 ) ) ;
#3160 = AXIS2_PLACEMENT_3D ( 'NONE', #3234, #3790, #6789 ) ;
#3161 = ORIENTED_EDGE ( 'NONE', *, *, #5301, .T. ) ;
#3162 = DIRECTION ( 'NONE',  ( 0.000000000000000000, 0.000000000000000000, 1.000000000000000000 ) ) ;
#3163 = CARTESIAN_POINT ( 'NONE',  ( 0.000000000000000000, 60.99999999999999289, 0.000000000000000000 ) ) ;
#3164 = AXIS2_PLACEMENT_3D ( 'NONE', #5067, #7385, #8219 ) ;
#3165 = EDGE_CURVE ( 'NONE', #9635, #7666, #257, .T. ) ;
#3166 = EDGE_CURVE ( 'NONE', #2152, #9475, #5637, .T. ) ;
#3167 = VERTEX_POINT ( 'NONE', #8699 ) ;
#3168 = CARTESIAN_POINT ( 'NONE',  ( -6.597235312685899800, 59.03111057313397225, 35.34929737147492546 ) ) ;
#3169 = EDGE_CURVE ( 'NONE', #5882, #6521, #3411, .T. ) ;
#3170 = ORIENTED_EDGE ( 'NONE', *, *, #7689, .T. ) ;
#3171 = ORIENTED_EDGE ( 'NONE', *, *, #3652, .F. ) ;
#3172 = FACE_OUTER_BOUND ( 'NONE', #9211, .T. ) ;
#3173 = FILL_AREA_STYLE ('',( #7726 ) ) ;
#3174 = AXIS2_PLACEMENT_3D ( 'NONE', #8229, #832, #5374 ) ;
#3175 = DIRECTION ( 'NONE',  ( -1.084202172485503325E-16, 0.000000000000000000, -1.000000000000000000 ) ) ;
#3176 = ORIENTED_EDGE ( 'NONE', *, *, #2251, .F. ) ;
#3177 = DIRECTION ( 'NONE',  ( -0.000000000000000000, 1.000000000000000000, -0.000000000000000000 ) ) ;
#3178 = PLANE ( 'NONE',  #4104 ) ;
#3179 = CARTESIAN_POINT ( 'NONE',  ( -3.850561375233625849, 59.53730689706332413, 34.89414954626303000 ) ) ;
#3180 = ORIENTED_EDGE ( 'NONE', *, *, #8292, .F. ) ;
#3181 = DIRECTION ( 'NONE',  ( -1.820952055660014662E-28, -1.000000000000000000, -7.038118388768679669E-30 ) ) ;
#3182 = VECTOR ( 'NONE', #9042, 1000.000000000000341 ) ;
#3183 = DIRECTION ( 'NONE',  ( 0.000000000000000000, -1.000000000000000000, 0.000000000000000000 ) ) ;
#3184 = FACE_OUTER_BOUND ( 'NONE', #3036, .T. ) ;
#3185 = CARTESIAN_POINT ( 'NONE',  ( 5.886704555688092810, 16.74912705918251987, 38.55424405853467817 ) ) ;
#3186 = LINE ( 'NONE', #1664, #2366 ) ;
#3187 = EDGE_LOOP ( 'NONE', ( #1746, #9733, #5763, #2026 ) ) ;
#3188 = CARTESIAN_POINT ( 'NONE',  ( -33.06426808735054124, 60.99999999999999289, -5.562309845534586294 ) ) ;
#3189 = EDGE_CURVE ( 'NONE', #7616, #5781, #7757, .T. ) ;
#3190 = AXIS2_PLACEMENT_3D ( 'NONE', #7298, #6557, #2430 ) ;
#3191 = CARTESIAN_POINT ( 'NONE',  ( -2.304377683636468772E-13, 59.99999999999999289, 33.00000000000000711 ) ) ;
#3192 = DIRECTION ( 'NONE',  ( -0.9999981025415526359, 0.001843852981148144709, 0.0006285852992236709872 ) ) ;
#3193 = CARTESIAN_POINT ( 'NONE',  ( -5.371095444502437921, 60.99999999999999289, -34.07933880998933773 ) ) ;
#3194 = ORIENTED_EDGE ( 'NONE', *, *, #8845, .F. ) ;
#3195 = CARTESIAN_POINT ( 'NONE',  ( 0.000000000000000000, 4.653657836759941744E-16, -3.799999999999999378 ) ) ;
#3196 = VECTOR ( 'NONE', #575, 1000.000000000000114 ) ;
#3197 = ORIENTED_EDGE ( 'NONE', *, *, #7528, .T. ) ;
#3198 = LINE ( 'NONE', #7860, #9345 ) ;
#3199 = LINE ( 'NONE', #158, #7823 ) ;
#3200 = DIRECTION ( 'NONE',  ( -1.000000000000000000, -0.000000000000000000, -0.000000000000000000 ) ) ;
#3201 = ITEM_DEFINED_TRANSFORMATION ( 'NONE', 'NONE', #9645,  #6314 ) ;
#3202 = DIRECTION ( 'NONE',  ( 0.9449569463147374782, 1.387778780781445873E-15, 0.3271946967961528729 ) ) ;
#3203 = DIRECTION ( 'NONE',  ( 0.7849198975831889191, -0.000000000000000000, -0.6195972517514874989 ) ) ;
#3204 = VERTEX_POINT ( 'NONE', #6266 ) ;
#3205 = DIRECTION ( 'NONE',  ( -0.000000000000000000, -1.000000000000000000, -0.000000000000000000 ) ) ;
#3206 = EDGE_LOOP ( 'NONE', ( #3934, #6142 ) ) ;
#3207 = EDGE_CURVE ( 'NONE', #8853, #9742, #4347, .T. ) ;
#3208 = DIRECTION ( 'NONE',  ( -1.820952055660014662E-28, -1.000000000000000000, 6.508102468073347395E-30 ) ) ;
#3209 = B_SPLINE_CURVE_WITH_KNOTS ( 'NONE', 3,
 ( #3605, #2253, #2458, #3048, #4605, #6853, #9240, #3000 ),
 .UNSPECIFIED., .F., .F.,
 ( 4, 2, 2, 4 ),
 ( 0.007099638519839713072, 0.008372149287075639906, 0.009008404670693602456, 0.009644660054311566741 ),
 .UNSPECIFIED. ) ;
#3210 = CARTESIAN_POINT ( 'NONE',  ( -10.00000000000117595, 2.631365979993403048, 41.36423575989225299 ) ) ;
#3211 = AXIS2_PLACEMENT_3D ( 'NONE', #757, #6127, #2368 ) ;
#3212 = VECTOR ( 'NONE', #390, 1000.000000000000000 ) ;
#3213 =( REPRESENTATION_RELATIONSHIP ('NONE','NONE', #5841, #490 ) REPRESENTATION_RELATIONSHIP_WITH_TRANSFORMATION ( #8455 )SHAPE_REPRESENTATION_RELATIONSHIP( ) );
#3214 = ORIENTED_EDGE ( 'NONE', *, *, #1947, .F. ) ;
#3215 = CARTESIAN_POINT ( 'NONE',  ( 0.000000000000000000, 59.99999999999999289, 0.000000000000000000 ) ) ;
#3216 = VERTEX_POINT ( 'NONE', #4110 ) ;
#3217 = ORIENTED_EDGE ( 'NONE', *, *, #6066, .T. ) ;
#3218 = ORIENTED_EDGE ( 'NONE', *, *, #7886, .F. ) ;
#3219 = CARTESIAN_POINT ( 'NONE',  ( -9.346405976260257376, -0.3019310421636504649, 38.01899321338081705 ) ) ;
#3220 = EDGE_CURVE ( 'NONE', #7752, #504, #307, .T. ) ;
#3221 = ADVANCED_FACE ( 'NONE', ( #3305 ), #9292, .F. ) ;
#3222 = CARTESIAN_POINT ( 'NONE',  ( 0.000000000000000000, 30.00000000000000000, 0.000000000000000000 ) ) ;
#3223 = EDGE_CURVE ( 'NONE', #9229, #8986, #1503, .T. ) ;
#3224 = CARTESIAN_POINT ( 'NONE',  ( 31.11591804390324612, 60.99999999999999289, -4.904043666719942074 ) ) ;
#3225 = VERTEX_POINT ( 'NONE', #994 ) ;
#3226 = CARTESIAN_POINT ( 'NONE',  ( -5.999999999999998224, 27.42469319230601243, 31.00000000000000711 ) ) ;
#3227 = CARTESIAN_POINT ( 'NONE',  ( -3.619905045646665709, 59.65318172148985099, 34.64718077370495308 ) ) ;
#3228 = VECTOR ( 'NONE', #3991, 1000.000000000000000 ) ;
#3229 = ORIENTED_EDGE ( 'NONE', *, *, #646, .T. ) ;
#3230 = LINE ( 'NONE', #6285, #6793 ) ;
#3231 = LINE ( 'NONE', #6245, #5467 ) ;
#3232 = DIRECTION ( 'NONE',  ( 1.000000000000000000, 0.000000000000000000, -2.168404344971006649E-16 ) ) ;
#3233 = PLANE ( 'NONE',  #9634 ) ;
#3234 = CARTESIAN_POINT ( 'NONE',  ( 9.101986939180200354E-27, 50.00000000000032685, 2.962080254467568742E-28 ) ) ;
#3235 = VERTEX_POINT ( 'NONE', #8598 ) ;
#3236 = EDGE_CURVE ( 'NONE', #3019, #3425, #7956, .T. ) ;
#3237 = CARTESIAN_POINT ( 'NONE',  ( 1.257247067695987565E-26, 60.00000000000029843, -37.00000000000000711 ) ) ;
#3238 = AXIS2_PLACEMENT_3D ( 'NONE', #8197, #7460, #8946 ) ;
#3239 = AXIS2_PLACEMENT_3D ( 'NONE', #2422, #135, #717 ) ;
#3240 = EDGE_CURVE ( 'NONE', #9574, #7738, #6850, .T. ) ;
#3241 = VECTOR ( 'NONE', #7440, 1000.000000000000000 ) ;
#3242 = AXIS2_PLACEMENT_3D ( 'NONE', #5106, #5159, #6718 ) ;
#3243 = VECTOR ( 'NONE', #5299, 1000.000000000000341 ) ;
#3244 =( BOUNDED_SURFACE ( )  B_SPLINE_SURFACE ( 3, 2, ( 
 ( #6516, #3462, #2659 ),
 ( #6418, #420, #3420 ),
 ( #9632, #2020, #4364 ),
 ( #5148, #8704, #1245 ),
 ( #4307, #462, #2858 ),
 ( #3507, #6461, #5687 ),
 ( #2766, #9487, #2809 ),
 ( #8053, #2712, #560 ),
 ( #2112, #5788, #9448 ),
 ( #1928, #8800, #5733 ),
 ( #1979, #5873, #8894 ),
 ( #507, #4950, #2066 ),
 ( #6568, #5095, #7367 ),
 ( #8749, #7962, #9590 ),
 ( #5831, #8102, #8156 ),
 ( #1201, #5002, #1292 ),
 ( #3563, #1338, #1387 ),
 ( #605, #9538, #8012 ),
 ( #4406, #4259, #3607 ),
 ( #9045, #5238, #1532 ),
 ( #3755, #6655, #5964 ),
 ( #9678, #3657, #2903 ),
 ( #7415, #5922, #3857 ),
 ( #1586, #4552, #5391 ),
 ( #8250, #5289, #6805 ),
 ( #750, #2158, #797 ),
 ( #7564, #62, #8401 ),
 ( #8303, #5341, #3806 ),
 ( #4607, #3051, #7513 ),
 ( #8349, #7464, #6069 ),
 ( #6116, #650, #9100 ),
 ( #1477, #7611, #4502 ),
 ( #2256, #2311, #2201 ),
 ( #6857, #851, #6749 ),
 ( #6706, #1632, #122 ),
 ( #10, #3002, #6011 ),
 ( #3103, #8948, #3705 ),
 ( #5192, #8199, #9143 ),
 ( #1434, #9734, #2957 ),
 ( #8992, #6163, #902 ),
 ( #5535, #2550, #8646 ),
 ( #5633, #4107, #4655 ),
 ( #1039, #8593, #1769 ),
 ( #7662, #2499, #3913 ),
 ( #9289, #8545, #5441 ),
 ( #9194, #2409, #4058 ),
 ( #8453, #7862, #1085 ),
 ( #3252, #7102, #6904 ),
 ( #1685, #989, #7711 ),
 ( #161, #3151, #4704 ),
 ( #943, #351, #6262 ),
 ( #4798, #1826, #3955 ) ),
 .UNSPECIFIED., .F., .F., .F. ) 
 B_SPLINE_SURFACE_WITH_KNOTS ( ( 4, 2, 2, 2, 2, 2, 2, 2, 2, 2, 2, 2, 2, 2, 2, 2, 2, 2, 2, 2, 2, 2, 2, 2, 2, 4 ),
 ( 3, 3 ),
 ( 0.04726531707896113044, 0.04874235823767866793, 0.05021939939639619849, 0.05317348171383126654, 0.05465052287254880403, 0.05612756403126634153, 0.05908164634870140958, 0.06055868750741894013, 0.06203572866613647763, 0.06351276982485401512, 0.06498981098357155262, 0.06794389330100661373, 0.06942093445972415122, 0.07089797561844168872, 0.07385205793587676371, 0.07532909909459430120, 0.07680614025331183869, 0.07828318141202937619, 0.07976022257074691368, 0.08271430488818197480, 0.08419134604689951229, 0.08566838720561703591, 0.08862246952305211090, 0.09009951068176964839, 0.09157655184048718588, 0.09453063415792226087 ),
 ( 0.000000000000000000, 1.000000000000000000 ),
 .UNSPECIFIED. ) 
 GEOMETRIC_REPRESENTATION_ITEM ( )  RATIONAL_B_SPLINE_SURFACE ( (
 ( 1.000000000000000000, 0.7071071909622603791, 1.000000000000000000),
 ( 1.000000000000000000, 0.7071216684788621532, 1.000000000000000000),
 ( 1.000000000000000000, 0.7075267130853096775, 1.000000000000000000),
 ( 1.000000000000000000, 0.7091156140370702410, 1.000000000000000000),
 ( 1.000000000000000000, 0.7103097360554838646, 1.000000000000000000),
 ( 1.000000000000000000, 0.7149216248805696505, 1.000000000000000000),
 ( 1.000000000000000000, 0.7193697620773539247, 1.000000000000000000),
 ( 1.000000000000000000, 0.7275797806198590623, 1.000000000000000000),
 ( 1.000000000000000000, 0.7305845420014355218, 1.000000000000000000),
 ( 1.000000000000000000, 0.7369677174223107086, 1.000000000000000000),
 ( 1.000000000000000000, 0.7403163103353537222, 1.000000000000000000),
 ( 1.000000000000000000, 0.7506600275792891797, 1.000000000000000000),
 ( 1.000000000000000000, 0.7579512107779988739, 1.000000000000000000),
 ( 1.000000000000000000, 0.7688664121945819607, 1.000000000000000000),
 ( 1.000000000000000000, 0.7724869259326714310, 1.000000000000000000),
 ( 1.000000000000000000, 0.7794781267615982223, 1.000000000000000000),
 ( 1.000000000000000000, 0.7828668203034458983, 1.000000000000000000),
 ( 1.000000000000000000, 0.7893489739652082005, 1.000000000000000000),
 ( 1.000000000000000000, 0.7924426342044915694, 1.000000000000000000),
 ( 1.000000000000000000, 0.7982547573422374976, 1.000000000000000000),
 ( 1.000000000000000000, 0.8009870661436891970, 1.000000000000000000),
 ( 1.000000000000000000, 0.8083787752127222781, 1.000000000000000000),
 ( 1.000000000000000000, 0.8122306866419456428, 1.000000000000000000),
 ( 1.000000000000000000, 0.8161590539804731703, 1.000000000000000000),
 ( 1.000000000000000000, 0.8171599891451262199, 1.000000000000000000),
 ( 1.000000000000000000, 0.8184978691222959402, 1.000000000000000000),
 ( 1.000000000000000000, 0.8188263875099578426, 1.000000000000000000),
 ( 1.000000000000000000, 0.8187846005707258845, 1.000000000000000000),
 ( 1.000000000000000000, 0.8174048505046132007, 1.000000000000000000),
 ( 1.000000000000000000, 0.8133903365045817013, 1.000000000000000000),
 ( 1.000000000000000000, 0.8117167614377021057, 1.000000000000000000),
 ( 1.000000000000000000, 0.8078263697157368473, 1.000000000000000000),
 ( 1.000000000000000000, 0.8056055056598052655, 1.000000000000000000),
 ( 1.000000000000000000, 0.8006760202143063943, 1.000000000000000000),
 ( 1.000000000000000000, 0.7979672363511526312, 1.000000000000000000),
 ( 1.000000000000000000, 0.7921221611992056433, 1.000000000000000000),
 ( 1.000000000000000000, 0.7889678644669387841, 1.000000000000000000),
 ( 1.000000000000000000, 0.7791076940979192456, 1.000000000000000000),
 ( 1.000000000000000000, 0.7720256508000469253, 1.000000000000000000),
 ( 1.000000000000000000, 0.7611892740573897864, 1.000000000000000000),
 ( 1.000000000000000000, 0.7575416872336065977, 1.000000000000000000),
 ( 1.000000000000000000, 0.7502769197745564611, 1.000000000000000000),
 ( 1.000000000000000000, 0.7467060562589890038, 1.000000000000000000),
 ( 1.000000000000000000, 0.7363894265406839557, 1.000000000000000000),
 ( 1.000000000000000000, 0.7300094285789220372, 1.000000000000000000),
 ( 1.000000000000000000, 0.7218273080856705270, 1.000000000000000000),
 ( 1.000000000000000000, 0.7193219373239115866, 1.000000000000000000),
 ( 1.000000000000000000, 0.7149816326288559454, 1.000000000000000000),
 ( 1.000000000000000000, 0.7131353591592815011, 1.000000000000000000),
 ( 1.000000000000000000, 0.7086530176431308226, 1.000000000000000000),
 ( 1.000000000000000000, 0.7070745693947934063, 1.000000000000000000),
 ( 1.000000000000000000, 0.7071072458330266430, 1.000000000000000000) ) ) 
 REPRESENTATION_ITEM ( '' )  SURFACE ( )  );
#3245 = CARTESIAN_POINT ( 'NONE',  ( 1.075405720943667276E-26, 59.00000000000029843, 3.085339770908351837E-28 ) ) ;
#3246 = VERTEX_POINT ( 'NONE', #4802 ) ;
#3247 = DIRECTION ( 'NONE',  ( 0.000000000000000000, 1.000000000000000000, 0.000000000000000000 ) ) ;
#3248 = CARTESIAN_POINT ( 'NONE',  ( 5.562309845534588959, 49.99999999999999289, -35.56426808735054834 ) ) ;
#3249 = VERTEX_POINT ( 'NONE', #5583 ) ;
#3250 = CARTESIAN_POINT ( 'NONE',  ( -6.000000000000005329, -10.00000000000000533, -31.00000000000000711 ) ) ;
#3251 = LINE ( 'NONE', #5676, #1673 ) ;
#3252 = CARTESIAN_POINT ( 'NONE',  ( 3.432825031707446684, -11.20495311582498310, 38.85090753550943532 ) ) ;
#3253 = PLANE ( 'NONE',  #1674 ) ;
#3254 = ORIENTED_EDGE ( 'NONE', *, *, #3417, .F. ) ;
#3255 = EDGE_LOOP ( 'NONE', ( #6378, #8612, #9181, #9132 ) ) ;
#3256 = DIRECTION ( 'NONE',  ( 0.000000000000000000, 1.000000000000000000, 0.000000000000000000 ) ) ;
#3257 = VERTEX_POINT ( 'NONE', #214 ) ;
#3258 = CARTESIAN_POINT ( 'NONE',  ( -31.00000000000000711, -10.00000000000000533, -5.999999999999996447 ) ) ;
#3259 = ORIENTED_EDGE ( 'NONE', *, *, #4085, .T. ) ;
#3260 = CARTESIAN_POINT ( 'NONE',  ( 30.12488991936162464, 28.28385863652524179, 6.000000000000000000 ) ) ;
#3261 = DIRECTION ( 'NONE',  ( 0.000000000000000000, 1.000000000000000000, 0.000000000000000000 ) ) ;
#3262 = ORIENTED_EDGE ( 'NONE', *, *, #6293, .T. ) ;
#3263 = CYLINDRICAL_SURFACE ( 'NONE', #9553, 4.500000000000005329 ) ;
#3264 = VERTEX_POINT ( 'NONE', #7808 ) ;
#3265 = DIRECTION ( 'NONE',  ( 0.9860132971832693549, 1.788557213313974126E-28, -0.1666666666666657970 ) ) ;
#3266 = ORIENTED_EDGE ( 'NONE', *, *, #2191, .T. ) ;
#3267 = ORIENTED_EDGE ( 'NONE', *, *, #5478, .F. ) ;
#3268 = CARTESIAN_POINT ( 'NONE',  ( -8.802338400919726524, -7.957579170021067405, 37.99520874873245901 ) ) ;
#3269 = CARTESIAN_POINT ( 'NONE',  ( 4.776122516674679455E-15, -15.00000000000000000, -39.00000000000002132 ) ) ;
#3270 = EDGE_CURVE ( 'NONE', #7710, #5104, #9440, .T. ) ;
#3271 = CARTESIAN_POINT ( 'NONE',  ( 8.673617379884035472E-16, 0.000000000000000000, 0.000000000000000000 ) ) ;
#3272 = ORIENTED_EDGE ( 'NONE', *, *, #4797, .F. ) ;
#3273 = FACE_OUTER_BOUND ( 'NONE', #6199, .T. ) ;
#3274 = EDGE_CURVE ( 'NONE', #3464, #7275, #8124, .T. ) ;
#3275 = ORIENTED_EDGE ( 'NONE', *, *, #2500, .T. ) ;
#3276 = DIRECTION ( 'NONE',  ( -0.000000000000000000, -1.000000000000000000, -0.000000000000000000 ) ) ;
#3277 = EDGE_CURVE ( 'NONE', #8953, #9301, #3601, .T. ) ;
#3278 = DIRECTION ( 'NONE',  ( -0.000000000000000000, 1.000000000000000000, -0.000000000000000000 ) ) ;
#3279 = DIRECTION ( 'NONE',  ( 0.000000000000000000, -0.000000000000000000, 1.000000000000000000 ) ) ;
#3280 = FILL_AREA_STYLE_COLOUR ( '', #498 ) ;
#3281 = CARTESIAN_POINT ( 'NONE',  ( 0.000000000000000000, 38.99999999999993605, 17.99999999999999645 ) ) ;
#3282 = EDGE_CURVE ( 'NONE', #1736, #5322, #3872, .T. ) ;
#3283 = CARTESIAN_POINT ( 'NONE',  ( -9.815840903884557989, 39.99999999999999289, 28.34870838944214455 ) ) ;
#3284 = EDGE_CURVE ( 'NONE', #5419, #4022, #4356, .T. ) ;
#3285 = ADVANCED_FACE ( 'NONE', ( #5035, #502, #5727, #9482, #1191, #8743 ), #5140, .T. ) ;
#3286 = AXIS2_PLACEMENT_3D ( 'NONE', #4235, #4326, #4919 ) ;
#3287 = EDGE_CURVE ( 'NONE', #2731, #8853, #4300, .T. ) ;
#3288 = VERTEX_POINT ( 'NONE', #4210 ) ;
#3289 = DIRECTION ( 'NONE',  ( -0.3271946967961528174, 0.000000000000000000, 0.9449569463147374782 ) ) ;
#3290 = CARTESIAN_POINT ( 'NONE',  ( -8.216777476527294510, 51.50000000000032685, -23.61111111111107519 ) ) ;
#3291 = EDGE_CURVE ( 'NONE', #4557, #179, #877, .T. ) ;
#3292 = ORIENTED_EDGE ( 'NONE', *, *, #526, .F. ) ;
#3293 = CARTESIAN_POINT ( 'NONE',  ( 5.137569555611264605, 60.99999999999999289, 34.09762842694627949 ) ) ;
#3294 = CARTESIAN_POINT ( 'NONE',  ( 0.000000000000000000, 54.99999999999999289, 0.000000000000000000 ) ) ;
#3295 = ORIENTED_EDGE ( 'NONE', *, *, #9390, .F. ) ;
#3296 = CARTESIAN_POINT ( 'NONE',  ( -7.509415180676684898, 9.906480154215739020, 42.53495263954286543 ) ) ;
#3297 = FACE_OUTER_BOUND ( 'NONE', #3450, .T. ) ;
#3298 = CARTESIAN_POINT ( 'NONE',  ( 1.300000000000000044, 1.082531754730548856, 0.6250000000000006661 ) ) ;
#3299 = CIRCLE ( 'NONE', #3722, 2.500000000000002220 ) ;
#3300 = AXIS2_PLACEMENT_3D ( 'NONE', #1996, #7984, #9606 ) ;
#3301 = CARTESIAN_POINT ( 'NONE',  ( -31.11591804390328164, 60.99999999999999289, 4.904043666719710259 ) ) ;
#3302 = AXIS2_PLACEMENT_3D ( 'NONE', #746, #1336, #7414 ) ;
#3303 = PLANE ( 'NONE',  #5124 ) ;
#3304 = ORIENTED_EDGE ( 'NONE', *, *, #1124, .F. ) ;
#3305 = FACE_OUTER_BOUND ( 'NONE', #617, .T. ) ;
#3306 = EDGE_LOOP ( 'NONE', ( #3395, #5458, #8504, #6267 ) ) ;
#3307 = DIRECTION ( 'NONE',  ( 0.000000000000000000, 0.000000000000000000, -1.000000000000000000 ) ) ;
#3308 = ORIENTED_EDGE ( 'NONE', *, *, #9495, .T. ) ;
#3309 = AXIS2_PLACEMENT_3D ( 'NONE', #1163, #7180, #1216 ) ;
#3310 = PRODUCT_DEFINITION_SHAPE ( 'NONE', 'NONE',  #9758 ) ;
#3311 = FACE_OUTER_BOUND ( 'NONE', #4822, .T. ) ;
#3312 = EDGE_CURVE ( 'NONE', #6269, #8597, #7400, .T. ) ;
#3313 = LINE ( 'NONE', #7161, #4979 ) ;
#3314 = PRODUCT_DEFINITION_CONTEXT ( 'detailed design', #6802, 'design' ) ;
#3315 = AXIS2_PLACEMENT_3D ( 'NONE', #5169, #2089, #2138 ) ;
#3316 = ORIENTED_EDGE ( 'NONE', *, *, #7237, .T. ) ;
#3317 = DIRECTION ( 'NONE',  ( -0.000000000000000000, -1.000000000000000000, -0.000000000000000000 ) ) ;
#3318 = ORIENTED_EDGE ( 'NONE', *, *, #1549, .F. ) ;
#3319 = EDGE_LOOP ( 'NONE', ( #1390, #3514, #17, #9431, #1007, #7552 ) ) ;
#3320 = CARTESIAN_POINT ( 'NONE',  ( 0.000000000000000000, 39.99999999999999289, 0.000000000000000000 ) ) ;
#3321 = ORIENTED_EDGE ( 'NONE', *, *, #2674, .F. ) ;
#3322 = ORIENTED_EDGE ( 'NONE', *, *, #9330, .F. ) ;
#3323 = CARTESIAN_POINT ( 'NONE',  ( -9.915904358114350003, 4.630888946090288449, 41.40979624514990576 ) ) ;
#3324 = DIRECTION ( 'NONE',  ( 1.820952055660014662E-28, 1.000000000000000000, -6.508102468073347395E-30 ) ) ;
#3325 = LINE ( 'NONE', #8667, #4158 ) ;
#3326 = ORIENTED_EDGE ( 'NONE', *, *, #553, .F. ) ;
#3327 = LINE ( 'NONE', #7127, #7412 ) ;
#3328 = FACE_OUTER_BOUND ( 'NONE', #711, .T. ) ;
#3329 = CIRCLE ( 'NONE', #8859, 1.000000000000000888 ) ;
#3330 = CARTESIAN_POINT ( 'NONE',  ( 9.348208607970679651, -0.2712915440469981232, 41.70628801877622749 ) ) ;
#3331 = ORIENTED_EDGE ( 'NONE', *, *, #255, .T. ) ;
#3332 = EDGE_CURVE ( 'NONE', #3433, #2169, #2904, .T. ) ;
#3333 = CARTESIAN_POINT ( 'NONE',  ( -33.06426808735054124, 60.99999999999999289, -5.562309845534581854 ) ) ;
#3334 = DIRECTION ( 'NONE',  ( 0.000000000000000000, 0.000000000000000000, -1.000000000000000000 ) ) ;
#3335 = CARTESIAN_POINT ( 'NONE',  ( 1.555535097482682654E-26, 78.08723716182652197, -25.00000000000000000 ) ) ;
#3336 = DIRECTION ( 'NONE',  ( 1.820952055660014662E-28, 1.000000000000000000, -6.508102468073347395E-30 ) ) ;
#3337 = CARTESIAN_POINT ( 'NONE',  ( -30.00000000000001066, 39.99999999999999289, -3.252551416882082410E-13 ) ) ;
#3338 = LINE ( 'NONE', #3531, #8751 ) ;
#3339 = AXIS2_PLACEMENT_3D ( 'NONE', #6651, #8945, #647 ) ;
#3340 = VERTEX_POINT ( 'NONE', #1970 ) ;
#3341 = CARTESIAN_POINT ( 'NONE',  ( 5.137569555611264605, 60.99999999999999289, 34.09762842694627949 ) ) ;
#3342 = CARTESIAN_POINT ( 'NONE',  ( 8.233735698244310719E-27, 44.00000000000019895, -24.09806918451537072 ) ) ;
#3343 = ORIENTED_EDGE ( 'NONE', *, *, #4278, .F. ) ;
#3344 = FACE_OUTER_BOUND ( 'NONE', #3319, .T. ) ;
#3345 = DIRECTION ( 'NONE',  ( 0.000000000000000000, 1.000000000000000000, 0.000000000000000000 ) ) ;
#3346 = EDGE_LOOP ( 'NONE', ( #9107, #5455, #7688, #1092 ) ) ;
#3347 = CARTESIAN_POINT ( 'NONE',  ( 1.555535097482682654E-26, 78.08723716182652197, -25.00000000000000000 ) ) ;
#3348 = VECTOR ( 'NONE', #1135, 1000.000000000000000 ) ;
#3349 = EDGE_CURVE ( 'NONE', #6218, #22, #4400, .T. ) ;
#3350 = DIRECTION ( 'NONE',  ( -0.000000000000000000, 1.000000000000000000, -0.000000000000000000 ) ) ;
#3351 = EDGE_CURVE ( 'NONE', #2873, #8065, #5782, .T. ) ;
#3352 = EDGE_CURVE ( 'NONE', #2376, #2351, #2849, .T. ) ;
#3353 = CARTESIAN_POINT ( 'NONE',  ( -37.34143203299149860, 61.94837758590841759, -4.137096292553819055 ) ) ;
#3354 = DIRECTION ( 'NONE',  ( -1.820952055660014662E-28, -1.000000000000000000, -7.038118388768679669E-30 ) ) ;
#3355 = VECTOR ( 'NONE', #7322, 1000.000000000000000 ) ;
#3356 = CARTESIAN_POINT ( 'NONE',  ( 8.673617379884035472E-16, 0.000000000000000000, 4.000000000000004441 ) ) ;
#3357 = VECTOR ( 'NONE', #4197, 1000.000000000000000 ) ;
#3358 = ORIENTED_EDGE ( 'NONE', *, *, #7818, .F. ) ;
#3359 = DIRECTION ( 'NONE',  ( -0.000000000000000000, -1.000000000000000000, -0.000000000000000000 ) ) ;
#3360 = CARTESIAN_POINT ( 'NONE',  ( 27.56211685706808723, 61.99999999999999289, 15.25056439471416780 ) ) ;
#3361 = ORIENTED_EDGE ( 'NONE', *, *, #7270, .F. ) ;
#3362 = CARTESIAN_POINT ( 'NONE',  ( 0.000000000000000000, 54.99999999999999289, 0.000000000000000000 ) ) ;
#3363 = DIRECTION ( 'NONE',  ( 0.000000000000000000, 1.000000000000000000, 0.000000000000000000 ) ) ;
#3364 = DIRECTION ( 'NONE',  ( -0.9860132971832693549, -1.788557213313974126E-28, 0.1666666666666657970 ) ) ;
#3365 = EDGE_LOOP ( 'NONE', ( #625, #5333, #5634, #7729, #4615 ) ) ;
#3366 = ORIENTED_EDGE ( 'NONE', *, *, #6896, .F. ) ;
#3367 = DIRECTION ( 'NONE',  ( -0.000000000000000000, -1.000000000000000000, -0.000000000000000000 ) ) ;
#3368 = ORIENTED_EDGE ( 'NONE', *, *, #2317, .T. ) ;
#3369 = FACE_OUTER_BOUND ( 'NONE', #9359, .T. ) ;
#3370 = EDGE_LOOP ( 'NONE', ( #7116, #8619, #4183, #2747 ) ) ;
#3371 = ORIENTED_EDGE ( 'NONE', *, *, #6047, .T. ) ;
#3372 = CARTESIAN_POINT ( 'NONE',  ( -9.671299335021130261, 5.920905817192278597, 41.54023692788936017 ) ) ;
#3373 = CARTESIAN_POINT ( 'NONE',  ( 15.97678174684330799, 60.99999999999999289, -28.87459861216662205 ) ) ;
#3374 = DIRECTION ( 'NONE',  ( 0.000000000000000000, 0.000000000000000000, -1.000000000000000000 ) ) ;
#3375 = AXIS2_PLACEMENT_3D ( 'NONE', #3847, #8340, #1575 ) ;
#3376 = ORIENTED_EDGE ( 'NONE', *, *, #3649, .F. ) ;
#3377 = FACE_OUTER_BOUND ( 'NONE', #601, .T. ) ;
#3378 = EDGE_CURVE ( 'NONE', #1432, #3849, #1239, .T. ) ;
#3379 = ORIENTED_EDGE ( 'NONE', *, *, #8103, .T. ) ;
#3380 = DIRECTION ( 'NONE',  ( -0.07726494571055114724, 9.462226845072048778E-18, 0.9970105958134776181 ) ) ;
#3381 = CARTESIAN_POINT ( 'NONE',  ( 1.300000000000000044, 0.000000000000000000, 0.000000000000000000 ) ) ;
#3382 = CARTESIAN_POINT ( 'NONE',  ( 0.000000000000000000, -15.00000000000000000, 0.000000000000000000 ) ) ;
#3383 = CIRCLE ( 'NONE', #244, 5.000000000000000888 ) ;
#3384 = CARTESIAN_POINT ( 'NONE',  ( 13.16003951335063782, 1.062643319146125087, 36.71276424047989906 ) ) ;
#3385 = AXIS2_PLACEMENT_3D ( 'NONE', #3041, #4646, #9670 ) ;
#3386 = FACE_OUTER_BOUND ( 'NONE', #4037, .T. ) ;
#3387 = CARTESIAN_POINT ( 'NONE',  ( -29.24912810952613640, 29.14236109046821710, 6.000000000000009770 ) ) ;
#3388 = VECTOR ( 'NONE', #6753, 1000.000000000000227 ) ;
#3389 = VECTOR ( 'NONE', #1223, 1000.000000000000000 ) ;
#3390 = DIRECTION ( 'NONE',  ( -0.000000000000000000, -1.000000000000000000, -0.000000000000000000 ) ) ;
#3391 = ORIENTED_EDGE ( 'NONE', *, *, #3648, .F. ) ;
#3392 = CARTESIAN_POINT ( 'NONE',  ( -28.34870838944214455, 59.99999999999999289, -9.815840903884556212 ) ) ;
#3393 = LINE ( 'NONE', #2095, #5437 ) ;
#3394 = AXIS2_PLACEMENT_3D ( 'NONE', #4362, #9631, #9589 ) ;
#3395 = ORIENTED_EDGE ( 'NONE', *, *, #5657, .F. ) ;
#3396 = CARTESIAN_POINT ( 'NONE',  ( -8.545448575588398654, 43.00000000000019895, -24.55555555555570990 ) ) ;
#3397 = CARTESIAN_POINT ( 'NONE',  ( -5.562309845534584518, 60.99999999999999289, 33.06426808735054124 ) ) ;
#3398 = ORIENTED_EDGE ( 'NONE', *, *, #8007, .T. ) ;
#3399 = VECTOR ( 'NONE', #4586, 1000.000000000000000 ) ;
#3400 = DIRECTION ( 'NONE',  ( 1.000000000000000000, 0.000000000000000000, -1.224646799147353207E-16 ) ) ;
#3401 = AXIS2_PLACEMENT_3D ( 'NONE', #7555, #9134, #6794 ) ;
#3402 = CIRCLE ( 'NONE', #4203, 2.500000000000002220 ) ;
#3403 = B_SPLINE_CURVE_WITH_KNOTS ( 'NONE', 3,
 ( #4483, #9078, #9664, #3687, #6685, #6102, #4640, #5903, #7549, #7490, #975, #5996, #9026, #5268, #8281, #1517, #8931, #778, #4588, #3840, #6835, #97, #3086, #6146 ),
 .UNSPECIFIED., .F., .F.,
 ( 4, 2, 2, 2, 2, 2, 2, 2, 2, 2, 2, 4 ),
 ( 0.000000000000000000, 0.002184979252289450703, 0.004369958504578901407, 0.006554937756868352110, 0.007647427383013077895, 0.008193672196085440354, 0.008739917009157802813, 0.009832406635302527731, 0.01092489626144725265, 0.01310987551373670422, 0.01529485476602615579, 0.01747983401831560563 ),
 .UNSPECIFIED. ) ;
#3404 = CYLINDRICAL_SURFACE ( 'NONE', #2223, 27.00000000000000355 ) ;
#3405 = CARTESIAN_POINT ( 'NONE',  ( -37.13646476935431195, 61.98650506287648909, -3.627735144839754344 ) ) ;
#3406 = AXIS2_PLACEMENT_3D ( 'NONE', #3986, #3278, #6978 ) ;
#3407 = CIRCLE ( 'NONE', #4680, 2.500000000000002220 ) ;
#3408 = FACE_OUTER_BOUND ( 'NONE', #4399, .T. ) ;
#3409 = ADVANCED_FACE ( 'NONE', ( #8794 ), #1286, .F. ) ;
#3410 = ORIENTED_EDGE ( 'NONE', *, *, #6598, .F. ) ;
#3411 = LINE ( 'NONE', #3960, #7805 ) ;
#3412 = VERTEX_POINT ( 'NONE', #641 ) ;
#3413 = DIRECTION ( 'NONE',  ( 0.000000000000000000, 0.000000000000000000, 1.000000000000000000 ) ) ;
#3414 = EDGE_CURVE ( 'NONE', #2208, #279, #3645, .T. ) ;
#3415 = VERTEX_POINT ( 'NONE', #9672 ) ;
#3416=STYLED_ITEM('',(#9785),#9444);
#3417 = EDGE_CURVE ( 'NONE', #4234, #9299, #4786, .T. ) ;
#3418 = CARTESIAN_POINT ( 'NONE',  ( 0.000000000000000000, 0.7216878364870328300, 1.250000000000000000 ) ) ;
#3419 = FACE_OUTER_BOUND ( 'NONE', #3969, .T. ) ;
#3420 = CARTESIAN_POINT ( 'NONE',  ( 0.3468554216641324128, 13.29422992404367143, 43.99968164972226248 ) ) ;
#3421 = DIRECTION ( 'NONE',  ( -0.000000000000000000, -1.000000000000000000, -0.000000000000000000 ) ) ;
#3422 = ORIENTED_EDGE ( 'NONE', *, *, #592, .F. ) ;
#3423 = DIRECTION ( 'NONE',  ( 0.000000000000000000, 0.000000000000000000, 1.000000000000000000 ) ) ;
#3424 = EDGE_CURVE ( 'NONE', #7994, #517, #5821, .T. ) ;
#3425 = VERTEX_POINT ( 'NONE', #6003 ) ;
#3426 = DIRECTION ( 'NONE',  ( 0.000000000000000000, 0.000000000000000000, 1.000000000000000000 ) ) ;
#3427 = ORIENTED_EDGE ( 'NONE', *, *, #9520, .T. ) ;
#3428 = ORIENTED_EDGE ( 'NONE', *, *, #2081, .T. ) ;
#3429 = EDGE_CURVE ( 'NONE', #2569, #4952, #7604, .T. ) ;
#3430 = CARTESIAN_POINT ( 'NONE',  ( -8.989938151044675863, -1.132833736518202628, 41.88450937582585709 ) ) ;
#3431 = DIRECTION ( 'NONE',  ( -1.735493991486225972E-29, 6.508102468073347395E-30, 1.000000000000000000 ) ) ;
#3432 = DIRECTION ( 'NONE',  ( 0.000000000000000000, 0.000000000000000000, 1.000000000000000000 ) ) ;
#3433 = VERTEX_POINT ( 'NONE', #6109 ) ;
#3434 = FACE_OUTER_BOUND ( 'NONE', #1602, .T. ) ;
#3435 = ORIENTED_EDGE ( 'NONE', *, *, #464, .T. ) ;
#3436 = CARTESIAN_POINT ( 'NONE',  ( -18.58791755254458167, 39.99999999999999289, -23.54759692749571087 ) ) ;
#3437 = DIRECTION ( 'NONE',  ( -0.000000000000000000, -1.000000000000000000, -0.000000000000000000 ) ) ;
#3438 = CARTESIAN_POINT ( 'NONE',  ( 0.000000000000000000, 39.99999999999999289, 0.000000000000000000 ) ) ;
#3439 = CARTESIAN_POINT ( 'NONE',  ( 0.000000000000000000, 39.99999999999999289, 0.000000000000000000 ) ) ;
#3440 = DIRECTION ( 'NONE',  ( -0.000000000000000000, -1.000000000000000000, -0.000000000000000000 ) ) ;
#3441 = EDGE_CURVE ( 'NONE', #1074, #2338, #2305, .T. ) ;
#3442 = ORIENTED_EDGE ( 'NONE', *, *, #9410, .T. ) ;
#3443 = LINE ( 'NONE', #544, #6234 ) ;
#3444 = FACE_OUTER_BOUND ( 'NONE', #3489, .T. ) ;
#3445 = ORIENTED_EDGE ( 'NONE', *, *, #1360, .F. ) ;
#3446 = CARTESIAN_POINT ( 'NONE',  ( 1.040310318760209318E-26, 56.50000000000029843, -24.09806918451523217 ) ) ;
#3447 = DIRECTION ( 'NONE',  ( -1.000000000000000000, -0.000000000000000000, -0.000000000000000000 ) ) ;
#3448 = DIRECTION ( 'NONE',  ( -0.000000000000000000, -1.000000000000000000, -0.000000000000000000 ) ) ;
#3449 = DIRECTION ( 'NONE',  ( 1.000000000000000000, 0.000000000000000000, -2.168404344971006649E-16 ) ) ;
#3450 = EDGE_LOOP ( 'NONE', ( #1917, #1603, #2254, #5038 ) ) ;
#3451 = DIRECTION ( 'NONE',  ( -0.000000000000000000, 1.000000000000000000, -0.000000000000000000 ) ) ;
#3452 = ORIENTED_EDGE ( 'NONE', *, *, #8538, .T. ) ;
#3453 = CARTESIAN_POINT ( 'NONE',  ( -3.999999999999999112, 28.99999999999997158, 24.67792535850613334 ) ) ;
#3454 = CARTESIAN_POINT ( 'NONE',  ( -3.482215743441875233, -15.00000000000000000, 29.62396259739072946 ) ) ;
#3455 = EDGE_CURVE ( 'NONE', #874, #3412, #3850, .T. ) ;
#3456 = ORIENTED_EDGE ( 'NONE', *, *, #237, .F. ) ;
#3457 = DIRECTION ( 'NONE',  ( 0.000000000000000000, 0.000000000000000000, 1.000000000000000000 ) ) ;
#3458 = AXIS2_PLACEMENT_3D ( 'NONE', #210, #3200, #4847 ) ;
#3459 = LINE ( 'NONE', #2615, #5457 ) ;
#3460 = ADVANCED_FACE ( 'NONE', ( #8192 ), #9187, .F. ) ;
#3461 = EDGE_CURVE ( 'NONE', #4048, #5730, #1525, .T. ) ;
#3462 = CARTESIAN_POINT ( 'NONE',  ( 0.01529561594344277208, 13.29484127273988570, 38.99999809024075859 ) ) ;
#3463 = SHAPE_REPRESENTATION_RELATIONSHIP ( 'NONE' , 'NONE' ,  #2928, #6901 ) ;
#3464 = VERTEX_POINT ( 'NONE', #1426 ) ;
#3465 = PLANE ( 'NONE',  #9394 ) ;
#3466 = ORIENTED_EDGE ( 'NONE', *, *, #8609, .F. ) ;
#3467 = CARTESIAN_POINT ( 'NONE',  ( 0.000000000000000000, 0.000000000000000000, 0.000000000000000000 ) ) ;
#3468 = ORIENTED_EDGE ( 'NONE', *, *, #1126, .F. ) ;
#3469 = ORIENTED_EDGE ( 'NONE', *, *, #1676, .T. ) ;
#3470 = CARTESIAN_POINT ( 'NONE',  ( -0.2571447251526570721, 13.29524039329391627, 39.00006612239294412 ) ) ;
#3471 = FACE_OUTER_BOUND ( 'NONE', #6494, .T. ) ;
#3472 = DIRECTION ( 'NONE',  ( -1.000000000000000000, 0.000000000000000000, 0.000000000000000000 ) ) ;
#3473 = EDGE_CURVE ( 'NONE', #1358, #8367, #2950, .T. ) ;
#3474 = EDGE_CURVE ( 'NONE', #341, #4748, #1938, .T. ) ;
#3475 = AXIS2_PLACEMENT_3D ( 'NONE', #9752, #8220, #8773 ) ;
#3476 = EDGE_CURVE ( 'NONE', #5730, #7381, #2995, .T. ) ;
#3477 = EDGE_LOOP ( 'NONE', ( #4100, #7642, #4690, #3972, #2480, #5843, #6028 ) ) ;
#3478 = CARTESIAN_POINT ( 'NONE',  ( 11.80999999999999872, 0.000000000000000000, 2.000000000000000000 ) ) ;
#3479 = ORIENTED_EDGE ( 'NONE', *, *, #5778, .F. ) ;
#3480 = ORIENTED_EDGE ( 'NONE', *, *, #107, .T. ) ;
#3481 = PLANE ( 'NONE',  #4485 ) ;
#3482 = CYLINDRICAL_SURFACE ( 'NONE', #1260, 30.00000000000001066 ) ;
#3483 = CARTESIAN_POINT ( 'NONE',  ( 12.20502364804429263, -2.690346678627072663, 37.04198800656732260 ) ) ;
#3484 = DIRECTION ( 'NONE',  ( 0.000000000000000000, 0.000000000000000000, 1.000000000000000000 ) ) ;
#3485 = DIRECTION ( 'NONE',  ( 1.000000000000000000, 0.000000000000000000, 0.000000000000000000 ) ) ;
#3486 = VERTEX_POINT ( 'NONE', #2245 ) ;
#3487 = CARTESIAN_POINT ( 'NONE',  ( -32.71871059427212458, 59.95478203631535052, -8.044358145045414688 ) ) ;
#3488 = DIRECTION ( 'NONE',  ( 1.000000000000000000, 0.000000000000000000, 1.079383496163345602E-14 ) ) ;
#3489 = EDGE_LOOP ( 'NONE', ( #4662, #4209, #1880, #3254 ) ) ;
#3490 = CARTESIAN_POINT ( 'NONE',  ( 9.811457508686334330E-27, 52.00000000000031974, -24.09806918451527835 ) ) ;
#3491 = CARTESIAN_POINT ( 'NONE',  ( 9.860132971832495485, 59.99999999999999289, 28.33333333333341031 ) ) ;
#3492 = CARTESIAN_POINT ( 'NONE',  ( 4.653657836759942730E-15, 58.99999999999999289, 38.00000000000000711 ) ) ;
#3493 = CARTESIAN_POINT ( 'NONE',  ( 9.269115636346888714E-27, 44.00000000000019895, -26.00000000000015987 ) ) ;
#3494 = VECTOR ( 'NONE', #3653, 1000.000000000000000 ) ;
#3495 = AXIS2_PLACEMENT_3D ( 'NONE', #8633, #7845, #1662 ) ;
#3496 = B_SPLINE_CURVE_WITH_KNOTS ( 'NONE', 3,
 ( #5527, #7702, #9235, #8496, #1720, #7652, #9374, #934, #3906, #4741, #981, #9285, #6894, #6942, #155, #3144, #6158, #7746 ),
 .UNSPECIFIED., .F., .F.,
 ( 4, 2, 2, 2, 2, 2, 2, 2, 4 ),
 ( 0.003057178249550605680, 0.003880613475145725487, 0.004704048700740845294, 0.005527483926335964234, 0.006350919151931084042, 0.007174354377526204717, 0.007997789603121323657, 0.008821224828716443464, 0.009644660054311565006 ),
 .UNSPECIFIED. ) ;
#3497 = CARTESIAN_POINT ( 'NONE',  ( -15.97678174684350871, 61.99999999999999289, 28.87459861216650836 ) ) ;
#3498 = VERTEX_POINT ( 'NONE', #8342 ) ;
#3499 = CARTESIAN_POINT ( 'NONE',  ( -8.216777476527294510, 56.00000000000030553, -23.61111111111111427 ) ) ;
#3500 = CARTESIAN_POINT ( 'NONE',  ( -1.119899052094893266, -9.430686232357382792, 39.50984196849405805 ) ) ;
#3501 = VECTOR ( 'NONE', #2456, 1000.000000000000000 ) ;
#3502 = EDGE_LOOP ( 'NONE', ( #1762, #8256, #8302, #4866, #4523 ) ) ;
#3503 = CARTESIAN_POINT ( 'NONE',  ( 1.099474886651785204E-26, 54.50000000000031264, -25.00000000000000000 ) ) ;
#3504 = PLANE ( 'NONE',  #9552 ) ;
#3505 = VECTOR ( 'NONE', #3472, 1000.000000000000000 ) ;
#3506 = AXIS2_PLACEMENT_3D ( 'NONE', #7407, #555, #3554 ) ;
#3507 = CARTESIAN_POINT ( 'NONE',  ( 3.500479179565848309, 17.79940450863160351, 38.85213755562799065 ) ) ;
#3508 = DIRECTION ( 'NONE',  ( 1.000000000000000000, 0.000000000000000000, 0.000000000000000000 ) ) ;
#3509 = ORIENTED_EDGE ( 'NONE', *, *, #1126, .T. ) ;
#3510 = DIRECTION ( 'NONE',  ( 0.000000000000000000, 0.000000000000000000, 1.000000000000000000 ) ) ;
#3511 = DIRECTION ( 'NONE',  ( 0.000000000000000000, 0.000000000000000000, -1.000000000000000000 ) ) ;
#3512 = DIRECTION ( 'NONE',  ( 0.3271946967961529840, 0.000000000000000000, -0.9449569463147373671 ) ) ;
#3513 = ORIENTED_EDGE ( 'NONE', *, *, #4744, .F. ) ;
#3514 = ORIENTED_EDGE ( 'NONE', *, *, #6960, .T. ) ;
#3515 = ADVANCED_FACE ( 'NONE', ( #2193 ), #9137, .F. ) ;
#3516 = CARTESIAN_POINT ( 'NONE',  ( -0.5291093370860696643, 13.28508303421404158, 38.99834356000749125 ) ) ;
#3517 = AXIS2_PLACEMENT_3D ( 'NONE', #3271, #7684, #4575 ) ;
#3518 = CARTESIAN_POINT ( 'NONE',  ( 1.300000000000000044, -1.082531754730548190, -0.6250000000000002220 ) ) ;
#3519 = B_SPLINE_CURVE_WITH_KNOTS ( 'NONE', 3,
 ( #9510, #1945, #4968, #5805 ),
 .UNSPECIFIED., .F., .F.,
 ( 4, 4 ),
 ( 0.000000000000000000, 0.003679109433542032855 ),
 .UNSPECIFIED. ) ;
#3520 = DIRECTION ( 'NONE',  ( 0.000000000000000000, 0.000000000000000000, 1.000000000000000000 ) ) ;
#3521 = EDGE_LOOP ( 'NONE', ( #3469, #6225, #2034, #3018 ) ) ;
#3522 = FACE_OUTER_BOUND ( 'NONE', #5320, .T. ) ;
#3523 = ORIENTED_EDGE ( 'NONE', *, *, #3223, .F. ) ;
#3524 = DIRECTION ( 'NONE',  ( 0.000000000000000000, 1.000000000000000000, -0.000000000000000000 ) ) ;
#3525 = EDGE_CURVE ( 'NONE', #982, #156, #3143, .T. ) ;
#3526 = ADVANCED_FACE ( 'NONE', ( #6157 ), #6743, .T. ) ;
#3527 = DIRECTION ( 'NONE',  ( -1.820952055660014662E-28, -1.000000000000000000, -7.038118388768679669E-30 ) ) ;
#3528 = CARTESIAN_POINT ( 'NONE',  ( 6.000000000000007994, -15.00000000000000000, 26.32489316217636954 ) ) ;
#3529 = PLANE ( 'NONE',  #3475 ) ;
#3530 = EDGE_CURVE ( 'NONE', #3288, #1017, #1468, .T. ) ;
#3531 = CARTESIAN_POINT ( 'NONE',  ( 9.815840903884561541, 59.99999999999999289, -28.34870838944214100 ) ) ;
#3532 = AXIS2_PLACEMENT_3D ( 'NONE', #5623, #978, #2592 ) ;
#3533 = DIRECTION ( 'NONE',  ( -1.000000000000000000, 0.000000000000000000, 0.000000000000000000 ) ) ;
#3534 = CARTESIAN_POINT ( 'NONE',  ( 0.000000000000000000, 60.99999999999999289, 0.000000000000000000 ) ) ;
#3535 = VECTOR ( 'NONE', #6356, 1000.000000000000000 ) ;
#3536 = ORIENTED_EDGE ( 'NONE', *, *, #8678, .F. ) ;
#3537 = AXIS2_PLACEMENT_3D ( 'NONE', #3497, #4298, #499 ) ;
#3538 = DIRECTION ( 'NONE',  ( 0.000000000000000000, 1.000000000000000000, 0.000000000000000000 ) ) ;
#3539 = DIRECTION ( 'NONE',  ( 0.000000000000000000, -0.8660254037844387076, 0.5000000000000001110 ) ) ;
#3540 = EDGE_CURVE ( 'NONE', #8683, #5164, #845, .T. ) ;
#3541 = ORIENTED_EDGE ( 'NONE', *, *, #890, .F. ) ;
#3542 = DIRECTION ( 'NONE',  ( -1.820952055660014662E-28, -1.000000000000000000, 6.508102468073347395E-30 ) ) ;
#3543 = DIRECTION ( 'NONE',  ( -1.735493991486225972E-29, 6.508102468073347395E-30, 1.000000000000000000 ) ) ;
#3544 = ADVANCED_FACE ( 'NONE', ( #7558 ), #3095, .F. ) ;
#3545 = CARTESIAN_POINT ( 'NONE',  ( -11.07761026121387538, -4.999999999999996447, 37.39366993089406321 ) ) ;
#3546 = VECTOR ( 'NONE', #3512, 1000.000000000000114 ) ;
#3547 = LINE ( 'NONE', #2224, #47 ) ;
#3548 = MECHANICAL_DESIGN_GEOMETRIC_PRESENTATION_REPRESENTATION (  '', ( #1026 ), #6851 ) ;
#3549 = CIRCLE ( 'NONE', #5288, 2.500000000000002220 ) ;
#3550 = ORIENTED_EDGE ( 'NONE', *, *, #8177, .T. ) ;
#3551 = CARTESIAN_POINT ( 'NONE',  ( 0.000000000000000000, 30.00000000000000000, -29.00000000000000355 ) ) ;
#3552 = CIRCLE ( 'NONE', #7342, 28.99999999999995026 ) ;
#3553 = ORIENTED_EDGE ( 'NONE', *, *, #3907, .T. ) ;
#3554 = DIRECTION ( 'NONE',  ( 0.000000000000000000, 0.000000000000000000, -1.000000000000000000 ) ) ;
#3555 = CARTESIAN_POINT ( 'NONE',  ( 0.2508212505825567207, -9.470617022380011463, 39.52758568340708933 ) ) ;
#3556 = ORIENTED_EDGE ( 'NONE', *, *, #5581, .T. ) ;
#3557 = CARTESIAN_POINT ( 'NONE',  ( -8.545448575588386220, 53.00000000000031974, -24.55555555555562108 ) ) ;
#3558 = VECTOR ( 'NONE', #2309, 1000.000000000000114 ) ;
#3559 = VECTOR ( 'NONE', #9335, 1000.000000000000000 ) ;
#3560 = CARTESIAN_POINT ( 'NONE',  ( 1.300000000000000044, 0.7216878364870328300, -1.250000000000000000 ) ) ;
#3561 = DIRECTION ( 'NONE',  ( 0.000000000000000000, 1.000000000000000000, 0.000000000000000000 ) ) ;
#3562 = EDGE_CURVE ( 'NONE', #1238, #6156, #6698, .T. ) ;
#3563 = CARTESIAN_POINT ( 'NONE',  ( 10.82166066357773637, 12.02267635125024015, 37.46937041031875992 ) ) ;
#3564 = DIRECTION ( 'NONE',  ( 0.000000000000000000, 0.000000000000000000, 1.000000000000000000 ) ) ;
#3565 = VERTEX_POINT ( 'NONE', #3905 ) ;
#3566 = DIRECTION ( 'NONE',  ( -0.000000000000000000, -1.000000000000000000, -0.000000000000000000 ) ) ;
#3567 = VERTEX_POINT ( 'NONE', #788 ) ;
#3568 = CARTESIAN_POINT ( 'NONE',  ( 0.000000000000000000, 39.99999999999999289, 0.000000000000000000 ) ) ;
#3569 = ORIENTED_EDGE ( 'NONE', *, *, #509, .F. ) ;
#3570 = DIRECTION ( 'NONE',  ( -1.000000000000000000, -0.000000000000000000, -0.000000000000000000 ) ) ;
#3571 = CLOSED_SHELL ( 'NONE', ( #3591, #5739, #3975, #8531, #4457, #4293, #4762, #5177, #4016, #4192, #6841, #7211, #7353, #9723, #541, #8488, #4217, #118, #3098, #2314, #2016, #5809, #4440, #9679, #2383, #6604, #1171, #292, #4441, #3756, #3515, #5482, #6061, #705, #4939, #7999, #9271, #386 ) ) ;
#3572 = ORIENTED_EDGE ( 'NONE', *, *, #4388, .F. ) ;
#3573 = CARTESIAN_POINT ( 'NONE',  ( -3.849165636106636423, 12.55126050286880357, 38.86455347263002835 ) ) ;
#3574 = DIRECTION ( 'NONE',  ( -0.000000000000000000, -1.000000000000000000, -0.000000000000000000 ) ) ;
#3575 = CARTESIAN_POINT ( 'NONE',  ( 4.898587196589413815E-15, 52.29648987751954792, 40.00000000000000711 ) ) ;
#3576 = VECTOR ( 'NONE', #8552, 1000.000000000000000 ) ;
#3577 = ORIENTED_EDGE ( 'NONE', *, *, #8678, .T. ) ;
#3578 = LINE ( 'NONE', #9650, #4015 ) ;
#3579 = ORIENTED_EDGE ( 'NONE', *, *, #8788, .F. ) ;
#3580 = CARTESIAN_POINT ( 'NONE',  ( 29.00000000000000355, 28.99999999999997158, -4.000000000000007105 ) ) ;
#3581 = CARTESIAN_POINT ( 'NONE',  ( -33.06426808735054124, 61.99999999999999289, -1.062309845534581632 ) ) ;
#3582 = CARTESIAN_POINT ( 'NONE',  ( 0.000000000000000000, 0.000000000000000000, 0.000000000000000000 ) ) ;
#3583 = DIRECTION ( 'NONE',  ( -0.000000000000000000, 1.000000000000000000, -0.000000000000000000 ) ) ;
#3584 = EDGE_CURVE ( 'NONE', #9400, #7616, #6893, .T. ) ;
#3585 = LINE ( 'NONE', #4385, #3709 ) ;
#3586 = EDGE_CURVE ( 'NONE', #1101, #6057, #9090, .T. ) ;
#3587 = DIRECTION ( 'NONE',  ( -0.000000000000000000, -1.000000000000000000, -0.000000000000000000 ) ) ;
#3588 = ORIENTED_EDGE ( 'NONE', *, *, #2619, .T. ) ;
#3589 = DIRECTION ( 'NONE',  ( 0.000000000000000000, -0.000000000000000000, 1.000000000000000000 ) ) ;
#3590 = CARTESIAN_POINT ( 'NONE',  ( 1.300000000000000044, 1.443375672974065216, 1.084202172492522584E-16 ) ) ;
#3591 = ADVANCED_FACE ( 'NONE', ( #253 ), #2711, .T. ) ;
#3592 = EDGE_LOOP ( 'NONE', ( #6104, #9357, #6808, #4126 ) ) ;
#3593 = DIRECTION ( 'NONE',  ( 0.000000000000000000, 0.000000000000000000, 1.000000000000000000 ) ) ;
#3594 = DIRECTION ( 'NONE',  ( 0.000000000000000000, 0.000000000000000000, -1.000000000000000000 ) ) ;
#3595 = CARTESIAN_POINT ( 'NONE',  ( -8.545448575588393325, -1.754907365325649309E-27, -24.55555555555563529 ) ) ;
#3596 = ADVANCED_FACE ( 'NONE', ( #1816 ), #8882, .T. ) ;
#3597 = EDGE_CURVE ( 'NONE', #2973, #1345, #8242, .T. ) ;
#3598 =( REPRESENTATION_RELATIONSHIP ('NONE','NONE', #5841, #490 ) REPRESENTATION_RELATIONSHIP_WITH_TRANSFORMATION ( #7863 )SHAPE_REPRESENTATION_RELATIONSHIP( ) );
#3599 = CARTESIAN_POINT ( 'NONE',  ( -8.216777476527274970, 78.08723716182652197, -23.61111111111111427 ) ) ;
#3600 = EDGE_LOOP ( 'NONE', ( #9251, #3738, #281, #1341 ) ) ;
#3601 = LINE ( 'NONE', #2012, #404 ) ;
#3602 = CARTESIAN_POINT ( 'NONE',  ( -11.07761026121418269, -14.99999999999999645, 37.39366993089506508 ) ) ;
#3603 = ORIENTED_EDGE ( 'NONE', *, *, #2865, .T. ) ;
#3604 = DIRECTION ( 'NONE',  ( -0.000000000000000000, -1.000000000000000000, -0.000000000000000000 ) ) ;
#3605 = CARTESIAN_POINT ( 'NONE',  ( 5.562309845534932684, 61.83753588906734677, -37.56426808735049150 ) ) ;
#3606 = ORIENTED_EDGE ( 'NONE', *, *, #226, .T. ) ;
#3607 = CARTESIAN_POINT ( 'NONE',  ( 8.665545440270191691, 8.296323355523078646, 42.03691472828050024 ) ) ;
#3608 = DIRECTION ( 'NONE',  ( 0.000000000000000000, 0.000000000000000000, 1.000000000000000000 ) ) ;
#3609 = ORIENTED_EDGE ( 'NONE', *, *, #1241, .F. ) ;
#3610 = CARTESIAN_POINT ( 'NONE',  ( 8.673617379884035472E-16, 28.99999999999997158, 4.000000000000004441 ) ) ;
#3611 = ORIENTED_EDGE ( 'NONE', *, *, #7939, .T. ) ;
#3612 = CARTESIAN_POINT ( 'NONE',  ( 6.000000000000001776, 30.00000000000000000, -26.32489316217636954 ) ) ;
#3613 = ORIENTED_EDGE ( 'NONE', *, *, #5889, .F. ) ;
#3614 = DIRECTION ( 'NONE',  ( 0.000000000000000000, 0.000000000000000000, -1.000000000000000000 ) ) ;
#3615 = ORIENTED_EDGE ( 'NONE', *, *, #3274, .T. ) ;
#3616 = CARTESIAN_POINT ( 'NONE',  ( -1.355205547380036402, 13.21018532110894128, 38.98542963915694770 ) ) ;
#3617 = LINE ( 'NONE', #5935, #8286 ) ;
#3618 = FACE_OUTER_BOUND ( 'NONE', #8900, .T. ) ;
#3619 = AXIS2_PLACEMENT_3D ( 'NONE', #1705, #4723, #3831 ) ;
#3620 = VECTOR ( 'NONE', #4382, 1000.000000000000000 ) ;
#3621 = ORIENTED_EDGE ( 'NONE', *, *, #6046, .T. ) ;
#3622 = FACE_OUTER_BOUND ( 'NONE', #3072, .T. ) ;
#3623 = VECTOR ( 'NONE', #2589, 1000.000000000000000 ) ;
#3624 = VERTEX_POINT ( 'NONE', #5432 ) ;
#3625 = CARTESIAN_POINT ( 'NONE',  ( 0.000000000000000000, 59.99999999999999289, 0.000000000000000000 ) ) ;
#3626 = DIRECTION ( 'NONE',  ( -0.1666666666666658525, -3.897465909857536228E-29, -0.9860132971832695770 ) ) ;
#3627 = CARTESIAN_POINT ( 'NONE',  ( 1.084683744678891232E-26, 53.50000000000031264, -25.00000000000000000 ) ) ;
#3628 = DIRECTION ( 'NONE',  ( 0.7849198975831886971, 0.000000000000000000, -0.6195972517514877209 ) ) ;
#3629 = VECTOR ( 'NONE', #142, 1000.000000000000000 ) ;
#3630 = EDGE_CURVE ( 'NONE', #5938, #9184, #992, .T. ) ;
#3631 = CARTESIAN_POINT ( 'NONE',  ( 1.300000000000000044, 1.443375672974065216, 1.084202172492522584E-16 ) ) ;
#3632 = ORIENTED_EDGE ( 'NONE', *, *, #5051, .F. ) ;
#3633 = DIRECTION ( 'NONE',  ( 0.000000000000000000, 0.000000000000000000, 1.000000000000000000 ) ) ;
#3634 = DIRECTION ( 'NONE',  ( 1.735493991486225972E-29, -6.508102468073347395E-30, -1.000000000000000000 ) ) ;
#3635 = CIRCLE ( 'NONE', #645, 38.00000000000000711 ) ;
#3636 = DIRECTION ( 'NONE',  ( 1.000000000000000000, 0.000000000000000000, -1.084202172485503448E-16 ) ) ;
#3637 = DIRECTION ( 'NONE',  ( 0.000000000000000000, -1.000000000000000000, 0.000000000000000000 ) ) ;
#3638 = CARTESIAN_POINT ( 'NONE',  ( 6.000000000000007994, -15.00000000000000000, 26.32489316217636954 ) ) ;
#3639 = CARTESIAN_POINT ( 'NONE',  ( 5.562309845534588959, 59.99999999999999289, -30.56426808735054479 ) ) ;
#3640 = AXIS2_PLACEMENT_3D ( 'NONE', #1414, #1374, #2149 ) ;
#3641 = DIRECTION ( 'NONE',  ( 1.820952055660014662E-28, 1.000000000000000000, 7.038118388768679669E-30 ) ) ;
#3642 = DIRECTION ( 'NONE',  ( 0.000000000000000000, 0.000000000000000000, -1.000000000000000000 ) ) ;
#3643 = VERTEX_POINT ( 'NONE', #2221 ) ;
#3644 = EDGE_LOOP ( 'NONE', ( #9144, #2354, #6872, #7522 ) ) ;
#3645 = LINE ( 'NONE', #6646, #9040 ) ;
#3646 = CARTESIAN_POINT ( 'NONE',  ( 4.817195445441472934, -15.00000000000000000, 29.05788463129285049 ) ) ;
#3647 = ORIENTED_EDGE ( 'NONE', *, *, #5473, .T. ) ;
#3648 = EDGE_CURVE ( 'NONE', #7858, #1498, #7701, .T. ) ;
#3649 = EDGE_CURVE ( 'NONE', #8122, #6057, #1628, .T. ) ;
#3650 = EDGE_CURVE ( 'NONE', #4765, #5790, #2558, .T. ) ;
#3651 = AXIS2_PLACEMENT_3D ( 'NONE', #7995, #2005, #4981 ) ;
#3652 = EDGE_CURVE ( 'NONE', #7154, #9614, #222, .T. ) ;
#3653 = DIRECTION ( 'NONE',  ( -0.000000000000000000, 1.000000000000000000, -0.000000000000000000 ) ) ;
#3654 = CARTESIAN_POINT ( 'NONE',  ( -8.237197373723139648, -4.999999999999998224, 27.80554943579302574 ) ) ;
#3655 = FACE_OUTER_BOUND ( 'NONE', #7117, .T. ) ;
#3656 = ORIENTED_EDGE ( 'NONE', *, *, #6659, .F. ) ;
#3657 = CARTESIAN_POINT ( 'NONE',  ( 9.365275055118548408, 6.895755298401112121, 38.01574831787047515 ) ) ;
#3658 = APPLICATION_PROTOCOL_DEFINITION ( 'draft international standard', 'automotive_design', 1998, #6297 ) ;
#3659 = CIRCLE ( 'NONE', #6488, 37.99999999999999289 ) ;
#3660 = ORIENTED_EDGE ( 'NONE', *, *, #9410, .F. ) ;
#3661 = DIRECTION ( 'NONE',  ( -1.820952055660014662E-28, -1.000000000000000000, -7.038118388768679669E-30 ) ) ;
#3662 = ORIENTED_EDGE ( 'NONE', *, *, #1988, .F. ) ;
#3663 = CARTESIAN_POINT ( 'NONE',  ( 34.72826512091049267, 59.61718548957851027, 3.689690490709788051 ) ) ;
#3664 = ORIENTED_EDGE ( 'NONE', *, *, #4032, .F. ) ;
#3665 = DIRECTION ( 'NONE',  ( 0.000000000000000000, 0.000000000000000000, 1.000000000000000000 ) ) ;
#3666 = VERTEX_POINT ( 'NONE', #8442 ) ;
#3667 = CARTESIAN_POINT ( 'NONE',  ( -1.077604443879617291, 13.24265641225903600, 38.99104434882794834 ) ) ;
#3668 = FACE_OUTER_BOUND ( 'NONE', #1425, .T. ) ;
#3669 = VECTOR ( 'NONE', #9069, 1000.000000000000000 ) ;
#3670 = CARTESIAN_POINT ( 'NONE',  ( -9.860132971832692661, 59.99999999999999289, -28.33333333333334281 ) ) ;
#3671 = ORIENTED_EDGE ( 'NONE', *, *, #3284, .T. ) ;
#3672 = CYLINDRICAL_SURFACE ( 'NONE', #652, 26.00000000000015987 ) ;
#3673 = ORIENTED_EDGE ( 'NONE', *, *, #3476, .F. ) ;
#3674 = AXIS2_PLACEMENT_3D ( 'NONE', #8021, #9458, #476 ) ;
#3675 = FACE_OUTER_BOUND ( 'NONE', #1116, .T. ) ;
#3676 =( LENGTH_UNIT ( ) NAMED_UNIT ( * ) SI_UNIT ( .MILLI., .METRE. ) );
#3677 = CARTESIAN_POINT ( 'NONE',  ( 8.283655523829511658E-27, 45.50000000000019185, 2.877339336914530364E-28 ) ) ;
#3678 = DIRECTION ( 'NONE',  ( -0.9860132971832693549, -1.788557213313974126E-28, 0.1666666666666657970 ) ) ;
#3679 = ADVANCED_FACE ( 'NONE', ( #4840 ), #7795, .F. ) ;
#3680 = DIRECTION ( 'NONE',  ( 1.735493991486225972E-29, -6.508102468073347395E-30, -1.000000000000000000 ) ) ;
#3681 = LINE ( 'NONE', #9172, #9153 ) ;
#3682 = VERTEX_POINT ( 'NONE', #3396 ) ;
#3683 = DIRECTION ( 'NONE',  ( -0.000000000000000000, 1.000000000000000000, -0.000000000000000000 ) ) ;
#3684 = CARTESIAN_POINT ( 'NONE',  ( -12.16083066526041989, 40.00000000000014921, -34.94444444444444287 ) ) ;
#3685 = DIRECTION ( 'NONE',  ( 0.000000000000000000, 0.000000000000000000, -1.000000000000000000 ) ) ;
#3686 = DIRECTION ( 'NONE',  ( 0.000000000000000000, 0.000000000000000000, -1.000000000000000000 ) ) ;
#3687 = CARTESIAN_POINT ( 'NONE',  ( 5.488653208922126048, -15.00000000000000000, 28.77476281181572304 ) ) ;
#3688 = FACE_OUTER_BOUND ( 'NONE', #7634, .T. ) ;
#3689 = EDGE_CURVE ( 'NONE', #7606, #2973, #4740, .T. ) ;
#3690 = DIRECTION ( 'NONE',  ( 0.000000000000000000, 1.000000000000000000, 1.224646799147353207E-16 ) ) ;
#3691 = AXIS2_PLACEMENT_3D ( 'NONE', #241, #6244, #8865 ) ;
#3692 = AXIS2_PLACEMENT_3D ( 'NONE', #9418, #2633, #6434 ) ;
#3693 = AXIS2_PLACEMENT_3D ( 'NONE', #4596, #7602, #9135 ) ;
#3694 = CARTESIAN_POINT ( 'NONE',  ( 9.754302352884585496E-27, 53.50000000000031264, 3.158525108795066799E-28 ) ) ;
#3695 = ORIENTED_EDGE ( 'NONE', *, *, #6944, .F. ) ;
#3696 = CARTESIAN_POINT ( 'NONE',  ( -29.00000000000000355, 28.99999999999997158, 0.000000000000000000 ) ) ;
#3697 = CARTESIAN_POINT ( 'NONE',  ( 10.07569075260316716, -15.00000000000064304, 37.15884857061433166 ) ) ;
#3698 = ORIENTED_EDGE ( 'NONE', *, *, #3455, .F. ) ;
#3699 = AXIS2_PLACEMENT_3D ( 'NONE', #5575, #6021, #5972 ) ;
#3700 = ADVANCED_FACE ( 'NONE', ( #3344 ), #7899, .F. ) ;
#3701 = CARTESIAN_POINT ( 'NONE',  ( 1.040310318760209318E-26, 51.50000000000032685, -25.00000000000000000 ) ) ;
#3702 = CARTESIAN_POINT ( 'NONE',  ( -8.545448575588372009, 57.50000000000029843, -24.55555555555557845 ) ) ;
#3703 = CARTESIAN_POINT ( 'NONE',  ( -23.54469556655647722, 39.99999999999999289, -29.82695610816121956 ) ) ;
#3704 = ORIENTED_EDGE ( 'NONE', *, *, #8310, .F. ) ;
#3705 = CARTESIAN_POINT ( 'NONE',  ( 8.477986360292581125, -2.018403734026263496, 42.12315275765950418 ) ) ;
#3706 = AXIS2_PLACEMENT_3D ( 'NONE', #7304, #5864, #457 ) ;
#3707 = ADVANCED_FACE ( 'NONE', ( #4699, #7745 ), #8640, .T. ) ;
#3708 = APPLICATION_PROTOCOL_DEFINITION ( 'draft international standard', 'automotive_design', 1998, #7836 ) ;
#3709 = VECTOR ( 'NONE', #4425, 1000.000000000000000 ) ;
#3710 = ORIENTED_EDGE ( 'NONE', *, *, #1553, .T. ) ;
#3711 = CARTESIAN_POINT ( 'NONE',  ( -24.67792535850613334, 0.000000000000000000, -3.999999999999997335 ) ) ;
#3712 = EDGE_CURVE ( 'NONE', #7580, #5699, #56, .T. ) ;
#3713 = ORIENTED_EDGE ( 'NONE', *, *, #6046, .F. ) ;
#3714 = CARTESIAN_POINT ( 'NONE',  ( 35.05384365671854852, 59.44855477671178079, 4.040090201280814419 ) ) ;
#3715 = ORIENTED_EDGE ( 'NONE', *, *, #9204, .F. ) ;
#3716 = LINE ( 'NONE', #3058, #3243 ) ;
#3717 = EDGE_CURVE ( 'NONE', #2001, #3754, #933, .T. ) ;
#3718 = VERTEX_POINT ( 'NONE', #6988 ) ;
#3719 = VECTOR ( 'NONE', #1876, 1000.000000000000000 ) ;
#3720 = CARTESIAN_POINT ( 'NONE',  ( 0.000000000000000000, 1.000000000000014655, -17.99999999999999645 ) ) ;
#3721 = CARTESIAN_POINT ( 'NONE',  ( 0.000000000000000000, -4.999999999999997335, 0.000000000000000000 ) ) ;
#3722 = AXIS2_PLACEMENT_3D ( 'NONE', #7165, #2662, #7589 ) ;
#3723 = AXIS2_PLACEMENT_3D ( 'NONE', #615, #4272, #7377 ) ;
#3724 = LINE ( 'NONE', #2821, #7296 ) ;
#3725 = ADVANCED_FACE ( 'NONE', ( #547 ), #8784, .F. ) ;
#3726 = CIRCLE ( 'NONE', #7348, 38.00000000000000711 ) ;
#3727 = ORIENTED_EDGE ( 'NONE', *, *, #1788, .T. ) ;
#3728 = CARTESIAN_POINT ( 'NONE',  ( -7.856683717344203011, 59.59863544270933744, 34.07748394475225950 ) ) ;
#3729 = EDGE_CURVE ( 'NONE', #1008, #7461, #9476, .T. ) ;
#3730 = LINE ( 'NONE', #7384, #942 ) ;
#3731 = DIRECTION ( 'NONE',  ( -1.820952055660014662E-28, -1.000000000000000000, -7.038118388768679669E-30 ) ) ;
#3732 = CIRCLE ( 'NONE', #4997, 2.500000000000002220 ) ;
#3733 = APPLICATION_CONTEXT ( 'automotive_design' ) ;
#3734 = DIRECTION ( 'NONE',  ( 0.000000000000000000, 0.000000000000000000, 1.000000000000000000 ) ) ;
#3735 = DIRECTION ( 'NONE',  ( 0.000000000000000000, 0.000000000000000000, 1.000000000000000000 ) ) ;
#3736 = EDGE_CURVE ( 'NONE', #6350, #1456, #2841, .T. ) ;
#3737 = DIRECTION ( 'NONE',  ( 0.000000000000000000, 0.000000000000000000, 1.000000000000000000 ) ) ;
#3738 = ORIENTED_EDGE ( 'NONE', *, *, #8889, .F. ) ;
#3739 = CARTESIAN_POINT ( 'NONE',  ( 0.000000000000000000, 13.29485247664129766, 300.0000000000000000 ) ) ;
#3740 = DIRECTION ( 'NONE',  ( 0.000000000000000000, 1.000000000000000000, 0.000000000000000000 ) ) ;
#3741 = DIRECTION ( 'NONE',  ( 0.000000000000000000, 0.000000000000000000, 1.000000000000000000 ) ) ;
#3742 = DIRECTION ( 'NONE',  ( 1.735493991486225972E-29, -6.508102468073347395E-30, -1.000000000000000000 ) ) ;
#3743 = AXIS2_PLACEMENT_3D ( 'NONE', #2837, #447, #2744 ) ;
#3744 = CARTESIAN_POINT ( 'NONE',  ( 0.000000000000000000, 59.99999999999999289, 0.000000000000000000 ) ) ;
#3745 = EDGE_CURVE ( 'NONE', #6660, #2267, #4394, .T. ) ;
#3746 = DIRECTION ( 'NONE',  ( -0.000000000000000000, -0.5000000000000002220, 0.8660254037844384856 ) ) ;
#3747 = DIRECTION ( 'NONE',  ( 0.000000000000000000, 0.000000000000000000, 1.000000000000000000 ) ) ;
#3748 = ORIENTED_EDGE ( 'NONE', *, *, #6649, .T. ) ;
#3749 = DIRECTION ( 'NONE',  ( 0.000000000000000000, -0.000000000000000000, -1.000000000000000000 ) ) ;
#3750 = CARTESIAN_POINT ( 'NONE',  ( 9.221621761046556287, -6.210574730312896641, 37.98076581590148493 ) ) ;
#3751 = VERTEX_POINT ( 'NONE', #5128 ) ;
#3752 = LINE ( 'NONE', #4499, #2710 ) ;
#3753 = CARTESIAN_POINT ( 'NONE',  ( 0.02451486836956002016, 18.29482697815588566, 38.99999229514322252 ) ) ;
#3754 = VERTEX_POINT ( 'NONE', #1324 ) ;
#3755 = CARTESIAN_POINT ( 'NONE',  ( 12.11803679389154453, 9.485944279750869512, 37.06999036926945479 ) ) ;
#3756 = ADVANCED_FACE ( 'NONE', ( #7197 ), #629, .F. ) ;
#3757 = ORIENTED_EDGE ( 'NONE', *, *, #2444, .F. ) ;
#3758 = CARTESIAN_POINT ( 'NONE',  ( -24.96033808169876878, 29.33187429063046991, -4.331874290630485014 ) ) ;
#3759 = LINE ( 'NONE', #3861, #631 ) ;
#3760 = CYLINDRICAL_SURFACE ( 'NONE', #4503, 26.00000000000009592 ) ;
#3761 = VERTEX_POINT ( 'NONE', #8689 ) ;
#3762 = CARTESIAN_POINT ( 'NONE',  ( 30.00000000000000711, 59.99999999999999289, 1.047444401652940259E-13 ) ) ;
#3763 = EDGE_LOOP ( 'NONE', ( #459, #8108, #6903, #3974, #5360 ) ) ;
#3764 = FACE_OUTER_BOUND ( 'NONE', #5628, .T. ) ;
#3765 = EDGE_CURVE ( 'NONE', #7319, #7328, #9668, .T. ) ;
#3766 = CARTESIAN_POINT ( 'NONE',  ( -2.568784777805515507, 60.99999999999999289, -16.29881421347316106 ) ) ;
#3767 = DIRECTION ( 'NONE',  ( 0.6195972517514877209, -0.000000000000000000, 0.7849198975831889191 ) ) ;
#3768 = ORIENTED_EDGE ( 'NONE', *, *, #2015, .T. ) ;
#3769 = CYLINDRICAL_SURFACE ( 'NONE', #3239, 30.00000000000000711 ) ;
#3770 = ORIENTED_EDGE ( 'NONE', *, *, #8179, .F. ) ;
#3771 = UNCERTAINTY_MEASURE_WITH_UNIT (LENGTH_MEASURE( 1.000000000000000082E-05 ), #4528, 'distance_accuracy_value', 'NONE');
#3772 = ORIENTED_EDGE ( 'NONE', *, *, #7514, .T. ) ;
#3773 = DIRECTION ( 'NONE',  ( 1.735493991486225972E-29, -6.508102468073347395E-30, -1.000000000000000000 ) ) ;
#3774 = DIRECTION ( 'NONE',  ( 0.000000000000000000, 0.000000000000000000, 1.000000000000000000 ) ) ;
#3775 = EDGE_CURVE ( 'NONE', #3682, #3950, #2404, .T. ) ;
#3776 = CARTESIAN_POINT ( 'NONE',  ( 1.221566888952841201E-22, 27.99999999999992184, -31.00000000000000711 ) ) ;
#3777 = EDGE_CURVE ( 'NONE', #8006, #5592, #8141, .T. ) ;
#3778 = ADVANCED_FACE ( 'NONE', ( #9615 ), #4344, .F. ) ;
#3779 = DIRECTION ( 'NONE',  ( -0.000000000000000000, -1.000000000000000000, -0.000000000000000000 ) ) ;
#3780 = AXIS2_PLACEMENT_3D ( 'NONE', #3156, #3007, #2411 ) ;
#3781 = CIRCLE ( 'NONE', #1, 38.00000000000000711 ) ;
#3782 = ORIENTED_EDGE ( 'NONE', *, *, #3584, .T. ) ;
#3783 = DIRECTION ( 'NONE',  ( 0.000000000000000000, 0.000000000000000000, 1.000000000000000000 ) ) ;
#3784 = ORIENTED_EDGE ( 'NONE', *, *, #7529, .T. ) ;
#3785 = CARTESIAN_POINT ( 'NONE',  ( -6.890850105526180158, 61.82663791069490600, 37.37679511928145359 ) ) ;
#3786 = DIRECTION ( 'NONE',  ( 1.820952055660014662E-28, 1.000000000000000000, 7.038118388768679669E-30 ) ) ;
#3787 = DIRECTION ( 'NONE',  ( -0.000000000000000000, -1.000000000000000000, -0.000000000000000000 ) ) ;
#3788 = DIRECTION ( 'NONE',  ( -0.000000000000000000, -0.000000000000000000, 1.000000000000000000 ) ) ;
#3789 = FILL_AREA_STYLE_COLOUR ( '', #8697 ) ;
#3790 = DIRECTION ( 'NONE',  ( -1.820952055660014662E-28, -1.000000000000000000, -7.038118388768679669E-30 ) ) ;
#3791 =( REPRESENTATION_RELATIONSHIP ('NONE','NONE', #5841, #5213 ) REPRESENTATION_RELATIONSHIP_WITH_TRANSFORMATION ( #6656 )SHAPE_REPRESENTATION_RELATIONSHIP( ) );
#3792 = EDGE_LOOP ( 'NONE', ( #24, #1953, #3835, #2074 ) ) ;
#3793 = AXIS2_PLACEMENT_3D ( 'NONE', #728, #9567, #2143 ) ;
#3794 = DIRECTION ( 'NONE',  ( 0.000000000000000000, 1.000000000000000000, 0.000000000000000000 ) ) ;
#3795 = VECTOR ( 'NONE', #8173, 1000.000000000000341 ) ;
#3796 = CARTESIAN_POINT ( 'NONE',  ( 9.860761315262647568E-27, 51.50000000000032685, -24.09806918451529612 ) ) ;
#3797 = DIRECTION ( 'NONE',  ( -0.000000000000000000, 1.000000000000000000, -0.000000000000000000 ) ) ;
#3798 = ORIENTED_EDGE ( 'NONE', *, *, #8889, .T. ) ;
#3799 = CARTESIAN_POINT ( 'NONE',  ( 0.000000000000000000, 58.99999999999999289, 0.000000000000000000 ) ) ;
#3800 = CARTESIAN_POINT ( 'NONE',  ( 6.498172386907730136, -14.99999999999968381, 36.82545492661441955 ) ) ;
#3801 = ORIENTED_EDGE ( 'NONE', *, *, #538, .T. ) ;
#3802 = PRESENTATION_LAYER_ASSIGNMENT (  '', '', ( #5848 ) ) ;
#3803 = DIRECTION ( 'NONE',  ( -0.000000000000000000, 1.000000000000000000, -0.000000000000000000 ) ) ;
#3804 = CARTESIAN_POINT ( 'NONE',  ( -6.000000000000005329, 28.28385863652523824, -30.12488991936162108 ) ) ;
#3805 = ORIENTED_EDGE ( 'NONE', *, *, #9701, .T. ) ;
#3806 = CARTESIAN_POINT ( 'NONE',  ( 9.998641156849346956, 2.615690621352292133, 41.36497489834112429 ) ) ;
#3807 = APPLICATION_PROTOCOL_DEFINITION ( 'draft international standard', 'automotive_design', 1998, #4296 ) ;
#3808 = ORIENTED_EDGE ( 'NONE', *, *, #7149, .T. ) ;
#3809 = CARTESIAN_POINT ( 'NONE',  ( 1.099474886651785204E-26, 54.50000000000031264, -25.00000000000000000 ) ) ;
#3810 = CARTESIAN_POINT ( 'NONE',  ( 8.677469957431129860E-27, 43.00000000000019895, -25.00000000000000000 ) ) ;
#3811 = CARTESIAN_POINT ( 'NONE',  ( 0.000000000000000000, -4.999999999999999112, -29.00000000000001776 ) ) ;
#3812 = ORIENTED_EDGE ( 'NONE', *, *, #480, .T. ) ;
#3813 = DIRECTION ( 'NONE',  ( 0.000000000000000000, 0.000000000000000000, 1.000000000000000000 ) ) ;
#3814 = ORIENTED_EDGE ( 'NONE', *, *, #7989, .F. ) ;
#3815 = CYLINDRICAL_SURFACE ( 'NONE', #2429, 2.500000000000002220 ) ;
#3816 = CARTESIAN_POINT ( 'NONE',  ( 0.000000000000000000, 0.000000000000000000, -27.99999999999999289 ) ) ;
#3817 = B_SPLINE_CURVE_WITH_KNOTS ( 'NONE', 3,
 ( #9057, #3210, #954, #3967, #7676, #4761, #2325, #6958, #9114, #808, #3818, #6083, #6221, #6129, #8509, #6915, #3922, #9254, #2467, #5503, #6761, #1547, #1739, #20 ),
 .UNSPECIFIED., .F., .F.,
 ( 4, 2, 2, 2, 2, 2, 2, 2, 2, 2, 2, 4 ),
 ( 0.04762592066223522019, 0.04960947359156670650, 0.05060125005623244271, 0.05159302652089818586, 0.05357657945022965829, 0.05556013237956113071, 0.05655190884422686692, 0.05754368530889261008, 0.05952723823822408250, 0.06051901470288982565, 0.06151079116755556186, 0.06349434409688703429 ),
 .UNSPECIFIED. ) ;
#3818 = CARTESIAN_POINT ( 'NONE',  ( -7.536685575068442056, -3.308866890532546012, 42.52863964422461862 ) ) ;
#3819 = CIRCLE ( 'NONE', #7123, 2.500000000000002220 ) ;
#3820 = ORIENTED_EDGE ( 'NONE', *, *, #2139, .F. ) ;
#3821 = CARTESIAN_POINT ( 'NONE',  ( -2.587326571347316140, -9.215009914112087586, 39.41319473361446057 ) ) ;
#3822 = PLANE ( 'NONE',  #4428 ) ;
#3823 = ORIENTED_EDGE ( 'NONE', *, *, #6249, .T. ) ;
#3824 = VERTEX_POINT ( 'NONE', #5769 ) ;
#3825 = CARTESIAN_POINT ( 'NONE',  ( -4.324486265735497881, -10.89814862554769803, 38.76179163200221467 ) ) ;
#3826 = VECTOR ( 'NONE', #5722, 1000.000000000000000 ) ;
#3827 = CYLINDRICAL_SURFACE ( 'NONE', #9397, 26.00000000000017408 ) ;
#3828 = CARTESIAN_POINT ( 'NONE',  ( -4.000000000000001776, 30.00000000000000000, 4.336808689942015271E-16 ) ) ;
#3829 = EDGE_LOOP ( 'NONE', ( #5113, #7685 ) ) ;
#3830 = LINE ( 'NONE', #3080, #3629 ) ;
#3831 = DIRECTION ( 'NONE',  ( 1.000000000000000000, 0.000000000000000000, 1.047444401652940007E-14 ) ) ;
#3832 = AXIS2_PLACEMENT_3D ( 'NONE', #3996, #4148, #1678 ) ;
#3833 = EDGE_CURVE ( 'NONE', #1089, #4910, #4450, .T. ) ;
#3834 = CARTESIAN_POINT ( 'NONE',  ( -4.249163891373062718, 59.35847319192267690, 35.19820543205469221 ) ) ;
#3835 = ORIENTED_EDGE ( 'NONE', *, *, #5056, .T. ) ;
#3836 = CARTESIAN_POINT ( 'NONE',  ( 9.460130474090460595, 0.03677082304110015909, 41.64927532210272432 ) ) ;
#3837 = DIRECTION ( 'NONE',  ( 1.000000000000000000, 0.000000000000000000, -2.168404344971006649E-16 ) ) ;
#3838 = ADVANCED_FACE ( 'NONE', ( #4290 ), #1959, .T. ) ;
#3839 = CYLINDRICAL_SURFACE ( 'NONE', #426, 2.500000000000002220 ) ;
#3840 = CARTESIAN_POINT ( 'NONE',  ( -4.822163095725295889, -14.99999999999999822, 29.05566526170479591 ) ) ;
#3841 = CARTESIAN_POINT ( 'NONE',  ( 28.34870838944214100, 59.99999999999999289, 9.815840903884559765 ) ) ;
#3842 = ORIENTED_EDGE ( 'NONE', *, *, #5826, .F. ) ;
#3843 = CARTESIAN_POINT ( 'NONE',  ( 5.423418723394456162E-28, -2.066522830327504070E-28, -26.00000000000011369 ) ) ;
#3844 = LINE ( 'NONE', #8883, #1102 ) ;
#3845 = EDGE_CURVE ( 'NONE', #1276, #6854, #5026, .T. ) ;
#3846 = PLANE ( 'NONE',  #1105 ) ;
#3847 = CARTESIAN_POINT ( 'NONE',  ( -31.00000000000000711, -15.00000000000000000, -5.999999999999996447 ) ) ;
#3848 = ADVANCED_FACE ( 'NONE', ( #7243 ), #495, .F. ) ;
#3849 = VERTEX_POINT ( 'NONE', #594 ) ;
#3850 = LINE ( 'NONE', #7651, #1464 ) ;
#3851 = CARTESIAN_POINT ( 'NONE',  ( 1.250417070894209948, -15.00000000000000000, 30.42002409700546650 ) ) ;
#3852 = ORIENTED_EDGE ( 'NONE', *, *, #4716, .T. ) ;
#3853 = DIRECTION ( 'NONE',  ( -0.000000000000000000, -1.000000000000000000, -0.000000000000000000 ) ) ;
#3854 = VECTOR ( 'NONE', #1717, 1000.000000000000000 ) ;
#3855 = DIRECTION ( 'NONE',  ( -1.735493991486225972E-29, 6.508102468073347395E-30, 1.000000000000000000 ) ) ;
#3856 = ORIENTED_EDGE ( 'NONE', *, *, #8234, .F. ) ;
#3857 = CARTESIAN_POINT ( 'NONE',  ( 9.680593967938868616, 5.886190330938374515, 41.53534638657208689 ) ) ;
#3858 = ORIENTED_EDGE ( 'NONE', *, *, #821, .T. ) ;
#3859 = DIRECTION ( 'NONE',  ( -0.000000000000000000, 1.000000000000000000, -0.000000000000000000 ) ) ;
#3860 = CONICAL_SURFACE ( 'NONE', #4969, 26.00000000000000355, 0.7853981633974346233 ) ;
#3861 = CARTESIAN_POINT ( 'NONE',  ( -8.216777476527294510, 50.50000000000031974, -23.61111111111111427 ) ) ;
#3862 = CARTESIAN_POINT ( 'NONE',  ( -28.33333333333344584, 39.99999999999999289, 9.860132971832394233 ) ) ;
#3863 = EDGE_LOOP ( 'NONE', ( #3954, #7242, #8198, #2782 ) ) ;
#3864 = LINE ( 'NONE', #8407, #7988 ) ;
#3865 = AXIS2_PLACEMENT_3D ( 'NONE', #552, #3451, #6453 ) ;
#3866 = ORIENTED_EDGE ( 'NONE', *, *, #6900, .T. ) ;
#3867 = CARTESIAN_POINT ( 'NONE',  ( -10.00000000000001599, 3.294852476658805873, 41.36423575989289247 ) ) ;
#3868 = PRODUCT ( 'MAS-312', 'MAS-312', '', ( #7416 ) ) ;
#3869 = CARTESIAN_POINT ( 'NONE',  ( 0.000000000000000000, 52.29648987751954792, 0.000000000000000000 ) ) ;
#3870 = EDGE_CURVE ( 'NONE', #4799, #5636, #6594, .T. ) ;
#3871 = CARTESIAN_POINT ( 'NONE',  ( 0.000000000000000000, 39.99999999999999289, 0.000000000000000000 ) ) ;
#3872 = CIRCLE ( 'NONE', #8445, 37.00000000000000711 ) ;
#3873 = VERTEX_POINT ( 'NONE', #6552 ) ;
#3874 = CARTESIAN_POINT ( 'NONE',  ( -4.904043666719616112, 60.99999999999999289, -31.11591804390330651 ) ) ;
#3875 = DIRECTION ( 'NONE',  ( 1.084202172485503325E-16, 0.000000000000000000, 1.000000000000000000 ) ) ;
#3876 = TOROIDAL_SURFACE ( 'NONE', #1667, 2.199999999999999734, 0.2000000000000000111 ) ;
#3877 = EDGE_LOOP ( 'NONE', ( #8886, #8898 ) ) ;
#3878 = AXIS2_PLACEMENT_3D ( 'NONE', #8014, #8848, #4264 ) ;
#3879 = VECTOR ( 'NONE', #3265, 1000.000000000000341 ) ;
#3880 = ORIENTED_EDGE ( 'NONE', *, *, #1672, .T. ) ;
#3881 = CIRCLE ( 'NONE', #1500, 34.49999999999999289 ) ;
#3882 = FACE_OUTER_BOUND ( 'NONE', #8268, .T. ) ;
#3883 = CARTESIAN_POINT ( 'NONE',  ( 12.43339847825378364, 54.99999999999999289, -35.90836395996003461 ) ) ;
#3884 = DIRECTION ( 'NONE',  ( -0.000000000000000000, 1.000000000000000000, -0.000000000000000000 ) ) ;
#3885 = CIRCLE ( 'NONE', #4522, 4.999999999999997335 ) ;
#3886 = CIRCLE ( 'NONE', #5145, 26.00000000000011369 ) ;
#3887 = VERTEX_POINT ( 'NONE', #2793 ) ;
#3888 = FACE_OUTER_BOUND ( 'NONE', #8164, .T. ) ;
#3889 = CARTESIAN_POINT ( 'NONE',  ( -8.545448575588396878, 50.00000000000032685, -24.55555555555564951 ) ) ;
#3890 = ADVANCED_FACE ( 'NONE', ( #5815 ), #8827, .F. ) ;
#3891 = CARTESIAN_POINT ( 'NONE',  ( 3.551870781420234824, -6.058861246625666830, 43.67865056495266884 ) ) ;
#3892 = CARTESIAN_POINT ( 'NONE',  ( 7.848671329280706210, 59.99999999999999289, -32.05305536707737701 ) ) ;
#3893 = CIRCLE ( 'NONE', #9414, 1.500000000000003109 ) ;
#3894 = FACE_OUTER_BOUND ( 'NONE', #8720, .T. ) ;
#3895 = CARTESIAN_POINT ( 'NONE',  ( -35.90836395996003461, 59.99999999999999289, -12.43339847825377475 ) ) ;
#3896 = CARTESIAN_POINT ( 'NONE',  ( 1.300000000000000044, -0.7216878364870318308, 1.250000000000000000 ) ) ;
#3897 = ORIENTED_EDGE ( 'NONE', *, *, #8796, .T. ) ;
#3898 = CLOSED_SHELL ( 'NONE', ( #431, #5580, #3890, #1849, #4758, #6419, #5465, #1528, #1934, #3001, #1254, #1509, #9689, #6964, #8787, #7769, #6610, #6038, #2554, #7675, #9746, #8939, #7485, #2661, #3285, #2739, #373, #2561, #2799, #1608, #5281, #1472, #296, #8091, #3707, #5877, #8833, #8548, #8967, #6472, #3221, #8413, #7260, #5355, #5001, #8777, #5048, #6187, #2000, #4808, #510, #4814, #3460, #2071, #1306, #8128, #6772 ) ) ;
#3899 = CARTESIAN_POINT ( 'NONE',  ( 0.000000000000000000, 59.99999999999999289, 0.000000000000000000 ) ) ;
#3900 = ADVANCED_FACE ( 'NONE', ( #2295 ), #9025, .T. ) ;
#3901 = AXIS2_PLACEMENT_3D ( 'NONE', #9616, #1132, #393 ) ;
#3902 = ORIENTED_EDGE ( 'NONE', *, *, #6785, .F. ) ;
#3903 = CARTESIAN_POINT ( 'NONE',  ( -9.082100980773482490, 61.99999999999999289, 35.86802812777740002 ) ) ;
#3904 = ORIENTED_EDGE ( 'NONE', *, *, #5656, .F. ) ;
#3905 = CARTESIAN_POINT ( 'NONE',  ( 31.16666666666668917, 59.99999999999999289, -10.84614626901589496 ) ) ;
#3906 = CARTESIAN_POINT ( 'NONE',  ( 37.45692540970868833, 61.81802411364413530, 6.576816292457711377 ) ) ;
#3907 = EDGE_CURVE ( 'NONE', #2298, #577, #2341, .T. ) ;
#3908 = ORIENTED_EDGE ( 'NONE', *, *, #4619, .F. ) ;
#3909 = ADVANCED_FACE ( 'NONE', ( #5325 ), #2148, .F. ) ;
#3910 = FACE_OUTER_BOUND ( 'NONE', #1208, .T. ) ;
#3911 = EDGE_CURVE ( 'NONE', #903, #8414, #198, .T. ) ;
#3912 = LINE ( 'NONE', #745, #6855 ) ;
#3913 = CARTESIAN_POINT ( 'NONE',  ( 5.006257199294086746, -5.386139767686431767, 43.36232512974734021 ) ) ;
#3914 = ITEM_DEFINED_TRANSFORMATION ( 'NONE', 'NONE', #4608,  #6314 ) ;
#3915 = ORIENTED_EDGE ( 'NONE', *, *, #1951, .T. ) ;
#3916 = CARTESIAN_POINT ( 'NONE',  ( 0.000000000000000000, 54.99999999999999289, 38.00000000000000711 ) ) ;
#3917 = PLANE ( 'NONE',  #5759 ) ;
#3918 = ORIENTED_EDGE ( 'NONE', *, *, #3417, .T. ) ;
#3919 = FACE_OUTER_BOUND ( 'NONE', #8691, .T. ) ;
#3920 = ORIENTED_EDGE ( 'NONE', *, *, #8991, .T. ) ;
#3921 = LINE ( 'NONE', #3115, #6556 ) ;
#3922 = CARTESIAN_POINT ( 'NONE',  ( -4.486453089411146067, -5.666157368122981097, 43.49188059297183173 ) ) ;
#3923 = APPLICATION_CONTEXT ( 'automotive_design' ) ;
#3924 = ORIENTED_EDGE ( 'NONE', *, *, #4335, .F. ) ;
#3925 = CARTESIAN_POINT ( 'NONE',  ( -4.080223084771134268, -8.820719837204659797, 39.23376499704423281 ) ) ;
#3926 = ORIENTED_EDGE ( 'NONE', *, *, #2969, .T. ) ;
#3927 = EDGE_LOOP ( 'NONE', ( #6326, #1585, #598, #8617, #2599 ) ) ;
#3928 = CARTESIAN_POINT ( 'NONE',  ( -1.339611196910782231, -6.636669372976692571, 43.96470529402514416 ) ) ;
#3929 = CARTESIAN_POINT ( 'NONE',  ( 0.000000000000000000, 30.00000000000000000, 0.000000000000000000 ) ) ;
#3930 = B_SPLINE_CURVE_WITH_KNOTS ( 'NONE', 3,
 ( #9128, #7032, #924, #6101, #2482, #9313, #5516, #2340, #9224, #9272, #4726, #6144, #5474, #287, #2438, #9177 ),
 .UNSPECIFIED., .F., .F.,
 ( 4, 2, 2, 2, 2, 2, 2, 4 ),
 ( 0.005084922178573566057, 0.006146119420698880481, 0.006676718041761534224, 0.007207316662824187967, 0.007737915283886840842, 0.008268513904949493717, 0.008799112526012148328, 0.009329711147074801203 ),
 .UNSPECIFIED. ) ;
#3931 = ORIENTED_EDGE ( 'NONE', *, *, #5776, .T. ) ;
#3932 = CARTESIAN_POINT ( 'NONE',  ( 31.18357922838635687, 59.99999999999999289, 10.79742499427301894 ) ) ;
#3933 = DIRECTION ( 'NONE',  ( -0.000000000000000000, -1.000000000000000000, -0.000000000000000000 ) ) ;
#3934 = ORIENTED_EDGE ( 'NONE', *, *, #7754, .T. ) ;
#3935 = DIRECTION ( 'NONE',  ( -1.735493991486225972E-29, 6.508102468073347395E-30, 1.000000000000000000 ) ) ;
#3936 = DIRECTION ( 'NONE',  ( -1.000000000000000000, -0.000000000000000000, -0.000000000000000000 ) ) ;
#3937 = DIRECTION ( 'NONE',  ( 0.000000000000000000, 0.000000000000000000, 1.000000000000000000 ) ) ;
#3938 = CARTESIAN_POINT ( 'NONE',  ( 3.229357168250672760, 17.86321051590875442, 38.87085120031289875 ) ) ;
#3939 = FACE_OUTER_BOUND ( 'NONE', #6860, .T. ) ;
#3940 = ORIENTED_EDGE ( 'NONE', *, *, #1898, .T. ) ;
#3941 = LINE ( 'NONE', #5379, #9067 ) ;
#3942 = VECTOR ( 'NONE', #5043, 1000.000000000000000 ) ;
#3943 = DIRECTION ( 'NONE',  ( 1.000000000000000000, 0.000000000000000000, -1.084202172485503448E-16 ) ) ;
#3944 = AXIS2_PLACEMENT_3D ( 'NONE', #6242, #4232, #2479 ) ;
#3945 = DIRECTION ( 'NONE',  ( -0.000000000000000000, 1.000000000000000000, -0.000000000000000000 ) ) ;
#3946 = EDGE_CURVE ( 'NONE', #6269, #8266, #1617, .T. ) ;
#3947 = EDGE_LOOP ( 'NONE', ( #3536, #7222, #1850, #2693 ) ) ;
#3948 = DIRECTION ( 'NONE',  ( -0.000000000000000000, -1.000000000000000000, -0.000000000000000000 ) ) ;
#3949 = LINE ( 'NONE', #4649, #2141 ) ;
#3950 = VERTEX_POINT ( 'NONE', #7444 ) ;
#3951 = DIRECTION ( 'NONE',  ( -1.820952055660014662E-28, -1.000000000000000000, -7.038118388768679669E-30 ) ) ;
#3952 = AXIS2_PLACEMENT_3D ( 'NONE', #9416, #2632, #5427 ) ;
#3953 = FACE_OUTER_BOUND ( 'NONE', #6742, .T. ) ;
#3954 = ORIENTED_EDGE ( 'NONE', *, *, #3166, .F. ) ;
#3955 = CARTESIAN_POINT ( 'NONE',  ( -0.01963426291157483600, -6.705128248126140278, 43.99999014335539016 ) ) ;
#3956 = CARTESIAN_POINT ( 'NONE',  ( 2.200000000000000178, 4.653657836759941744E-16, -3.799999999999999378 ) ) ;
#3957 = EDGE_CURVE ( 'NONE', #5836, #2719, #2699, .T. ) ;
#3958 = ADVANCED_FACE ( 'NONE', ( #5222 ), #5953, .F. ) ;
#3959 = CARTESIAN_POINT ( 'NONE',  ( -10.84614626901599799, 54.99999999999999289, -31.16666666666666785 ) ) ;
#3960 = CARTESIAN_POINT ( 'NONE',  ( 1.636886378333599496E-26, 78.08723716182652197, -37.00000000000000711 ) ) ;
#3961 = ORIENTED_EDGE ( 'NONE', *, *, #2808, .F. ) ;
#3962 = LINE ( 'NONE', #216, #8935 ) ;
#3963 = AXIS2_PLACEMENT_3D ( 'NONE', #582, #3583, #8919 ) ;
#3964 = EDGE_CURVE ( 'NONE', #3887, #5003, #9648, .T. ) ;
#3965 = EDGE_LOOP ( 'NONE', ( #5811, #1765, #4976, #4606 ) ) ;
#3966 = FACE_BOUND ( 'NONE', #7569, .T. ) ;
#3967 = CARTESIAN_POINT ( 'NONE',  ( -9.738952295719967012, 1.000838298946814087, 41.50427199400585465 ) ) ;
#3968 =( GEOMETRIC_REPRESENTATION_CONTEXT ( 3 ) GLOBAL_UNCERTAINTY_ASSIGNED_CONTEXT ( ( #5257 ) ) GLOBAL_UNIT_ASSIGNED_CONTEXT ( ( #7163, #465, #2660 ) ) REPRESENTATION_CONTEXT ( 'NONE', 'WORKASPACE' ) );
#3969 = EDGE_LOOP ( 'NONE', ( #3673, #1043, #7126, #2264 ) ) ;
#3970 = FACE_OUTER_BOUND ( 'NONE', #1002, .T. ) ;
#3971 = ORIENTED_EDGE ( 'NONE', *, *, #7518, .F. ) ;
#3972 = ORIENTED_EDGE ( 'NONE', *, *, #4088, .F. ) ;
#3973 = ORIENTED_EDGE ( 'NONE', *, *, #4862, .T. ) ;
#3974 = ORIENTED_EDGE ( 'NONE', *, *, #3124, .T. ) ;
#3975 = ADVANCED_FACE ( 'NONE', ( #3894 ), #1446, .T. ) ;
#3976 = PRODUCT_DEFINITION_FORMATION_WITH_SPECIFIED_SOURCE ( 'ANY', '', #3868, .NOT_KNOWN. ) ;
#3977 = CARTESIAN_POINT ( 'NONE',  ( -7.783452355770943853, -8.875924410859513003, 38.21717263769323836 ) ) ;
#3978 = DIRECTION ( 'NONE',  ( 0.000000000000000000, 0.000000000000000000, -1.000000000000000000 ) ) ;
#3979 = AXIS2_PLACEMENT_3D ( 'NONE', #7947, #8737, #1373 ) ;
#3980 = DIRECTION ( 'NONE',  ( 1.000000000000000000, 0.000000000000000000, -1.084202172485503325E-16 ) ) ;
#3981 = VERTEX_POINT ( 'NONE', #42 ) ;
#3982 = DIRECTION ( 'NONE',  ( -0.000000000000000000, 1.000000000000000000, -0.000000000000000000 ) ) ;
#3983 = ORIENTED_EDGE ( 'NONE', *, *, #1246, .T. ) ;
#3984 = DIRECTION ( 'NONE',  ( 0.000000000000000000, 1.000000000000000000, 0.000000000000000000 ) ) ;
#3985 = VECTOR ( 'NONE', #4066, 1000.000000000000000 ) ;
#3986 = CARTESIAN_POINT ( 'NONE',  ( 0.000000000000000000, 60.99999999999999289, 0.000000000000000000 ) ) ;
#3987 = CARTESIAN_POINT ( 'NONE',  ( 0.000000000000000000, 39.99999999999999289, 0.000000000000000000 ) ) ;
#3988 = DIRECTION ( 'NONE',  ( 0.000000000000000000, 0.000000000000000000, 1.000000000000000000 ) ) ;
#3989 = DIRECTION ( 'NONE',  ( 0.000000000000000000, 1.000000000000000000, 0.000000000000000000 ) ) ;
#3990 = ORIENTED_EDGE ( 'NONE', *, *, #4375, .T. ) ;
#3991 = DIRECTION ( 'NONE',  ( 1.735493991486225972E-29, -6.508102468073347395E-30, -1.000000000000000000 ) ) ;
#3992 = CIRCLE ( 'NONE', #2079, 30.00000000000001066 ) ;
#3993 = AXIS2_PLACEMENT_3D ( 'NONE', #1029, #7855, #1079 ) ;
#3994 = CARTESIAN_POINT ( 'NONE',  ( -18.51991245392837371, 3.294852476641298988, 294.6136752714472777 ) ) ;
#3995 = ORIENTED_EDGE ( 'NONE', *, *, #9217, .F. ) ;
#3996 = CARTESIAN_POINT ( 'NONE',  ( 0.000000000000000000, 58.99999999999999289, 0.000000000000000000 ) ) ;
#3997 = LINE ( 'NONE', #1080, #7192 ) ;
#3998 = VECTOR ( 'NONE', #4230, 1000.000000000000000 ) ;
#3999 = ORIENTED_EDGE ( 'NONE', *, *, #7201, .T. ) ;
#4000 = AXIS2_PLACEMENT_3D ( 'NONE', #3392, #3289, #6402 ) ;
#4001 = DIRECTION ( 'NONE',  ( -1.533293416683393860E-16, -0.7071067811865376918, -0.7071067811865573427 ) ) ;
#4002 = CARTESIAN_POINT ( 'NONE',  ( 0.000000000000000000, 60.99999999999999289, 0.000000000000000000 ) ) ;
#4003 = ORIENTED_EDGE ( 'NONE', *, *, #6485, .F. ) ;
#4004 = DIRECTION ( 'NONE',  ( 0.3286710990610922090, 6.289316826390952918E-29, 0.9444444444444435316 ) ) ;
#4005 = DIRECTION ( 'NONE',  ( -1.000000000000000000, 0.000000000000000000, 0.000000000000000000 ) ) ;
#4006 = ORIENTED_EDGE ( 'NONE', *, *, #7402, .T. ) ;
#4007 = CARTESIAN_POINT ( 'NONE',  ( 4.898587196589413815E-15, 30.99999999999998579, -40.00000000000000711 ) ) ;
#4008 = CARTESIAN_POINT ( 'NONE',  ( -31.11591804390328164, 60.99999999999999289, 4.904043666719710259 ) ) ;
#4009 = ADVANCED_FACE ( 'NONE', ( #4539 ), #8976, .F. ) ;
#4010 = EDGE_CURVE ( 'NONE', #9635, #2374, #3403, .T. ) ;
#4011 = ORIENTED_EDGE ( 'NONE', *, *, #7458, .F. ) ;
#4012 = CARTESIAN_POINT ( 'NONE',  ( 28.37252191822216218, 30.00000000000000000, 6.000000000000000000 ) ) ;
#4013 = DIRECTION ( 'NONE',  ( -0.000000000000000000, 1.000000000000000000, -0.000000000000000000 ) ) ;
#4014 = EDGE_CURVE ( 'NONE', #7168, #1933, #4831, .T. ) ;
#4015 = VECTOR ( 'NONE', #6671, 1000.000000000000000 ) ;
#4016 = ADVANCED_FACE ( 'NONE', ( #4040 ), #6932, .F. ) ;
#4017 = VECTOR ( 'NONE', #5130, 1000.000000000000000 ) ;
#4018 = CIRCLE ( 'NONE', #9534, 31.49999999999999289 ) ;
#4019 = EDGE_LOOP ( 'NONE', ( #7516, #7577 ) ) ;
#4020 = CARTESIAN_POINT ( 'NONE',  ( -8.545448575588418194, -1.752788842386823350E-27, -24.55555555555570990 ) ) ;
#4021 = EDGE_CURVE ( 'NONE', #6202, #9175, #4086, .T. ) ;
#4022 = VERTEX_POINT ( 'NONE', #4687 ) ;
#4023 = PLANE ( 'NONE',  #8922 ) ;
#4024 = EDGE_LOOP ( 'NONE', ( #5383, #7669, #695, #6241 ) ) ;
#4025 = ORIENTED_EDGE ( 'NONE', *, *, #4642, .F. ) ;
#4026 = CARTESIAN_POINT ( 'NONE',  ( -10.56205462419233498, -5.828843216915552183, 37.54361741745486114 ) ) ;
#4027 = CARTESIAN_POINT ( 'NONE',  ( -5.562309845534701758, 60.99999999999999289, 33.06426808735052703 ) ) ;
#4028 = AXIS2_PLACEMENT_3D ( 'NONE', #4530, #2042, #583 ) ;
#4029 = ADVANCED_FACE ( 'NONE', ( #971 ), #9183, .T. ) ;
#4030 = DIRECTION ( 'NONE',  ( -0.6195972517514871658, -0.000000000000000000, -0.7849198975831892522 ) ) ;
#4031 = EDGE_CURVE ( 'NONE', #4621, #4883, #5426, .T. ) ;
#4032 = EDGE_CURVE ( 'NONE', #7590, #4511, #4924, .T. ) ;
#4033 = ORIENTED_EDGE ( 'NONE', *, *, #4487, .T. ) ;
#4034 = DIRECTION ( 'NONE',  ( -1.820952055660014662E-28, -1.000000000000000000, -7.038118388768679669E-30 ) ) ;
#4035 = CIRCLE ( 'NONE', #719, 10.00000000000000178 ) ;
#4036 = CIRCLE ( 'NONE', #9550, 30.00000000000001066 ) ;
#4037 = EDGE_LOOP ( 'NONE', ( #7301, #8104, #2200, #5784 ) ) ;
#4038 = LINE ( 'NONE', #7075, #1284 ) ;
#4039 = CARTESIAN_POINT ( 'NONE',  ( 5.987883466156523227, 58.97190912209828895, -35.53684633323564412 ) ) ;
#4040 = FACE_OUTER_BOUND ( 'NONE', #3592, .T. ) ;
#4041 = DIRECTION ( 'NONE',  ( -1.000000000000000000, 0.000000000000000000, -3.083952846180987322E-15 ) ) ;
#4042 = CARTESIAN_POINT ( 'NONE',  ( 0.000000000000000000, 28.99999999999997158, 0.000000000000000000 ) ) ;
#4043 = VECTOR ( 'NONE', #5830, 1000.000000000000000 ) ;
#4044 = VECTOR ( 'NONE', #8658, 1000.000000000000000 ) ;
#4045 = CIRCLE ( 'NONE', #5307, 30.00000000000000711 ) ;
#4046 = VECTOR ( 'NONE', #659, 1000.000000000000000 ) ;
#4047 = DIRECTION ( 'NONE',  ( -0.000000000000000000, 1.000000000000000000, -0.000000000000000000 ) ) ;
#4048 = VERTEX_POINT ( 'NONE', #7786 ) ;
#4049 = CARTESIAN_POINT ( 'NONE',  ( 32.59762842694625817, 60.99999999999999289, -5.137569555611371186 ) ) ;
#4050 = DIRECTION ( 'NONE',  ( -1.000000000000000000, 0.000000000000000000, 2.168404344971006649E-16 ) ) ;
#4051 = EDGE_CURVE ( 'NONE', #3027, #294, #192, .T. ) ;
#4052 = VERTEX_POINT ( 'NONE', #1020 ) ;
#4053 = CARTESIAN_POINT ( 'NONE',  ( -6.000000000000005329, 27.42469319230600533, -31.00000000000000711 ) ) ;
#4054 = DIRECTION ( 'NONE',  ( 0.000000000000000000, 0.000000000000000000, -1.000000000000000000 ) ) ;
#4055 = VECTOR ( 'NONE', #1817, 1000.000000000000000 ) ;
#4056 = CARTESIAN_POINT ( 'NONE',  ( -36.28089590215267179, 61.98637676474528746, -8.721193672020515208 ) ) ;
#4057 = ORIENTED_EDGE ( 'NONE', *, *, #1902, .T. ) ;
#4058 = CARTESIAN_POINT ( 'NONE',  ( 3.525292369978886065, -6.068895536008623637, 43.68349390364525675 ) ) ;
#4059 = DIRECTION ( 'NONE',  ( -0.000000000000000000, 1.000000000000000000, -0.000000000000000000 ) ) ;
#4060 = ORIENTED_EDGE ( 'NONE', *, *, #5354, .T. ) ;
#4061 = ORIENTED_EDGE ( 'NONE', *, *, #3540, .F. ) ;
#4062 = CARTESIAN_POINT ( 'NONE',  ( 0.000000000000000000, 39.99999999999999289, 0.000000000000000000 ) ) ;
#4063 = ORIENTED_EDGE ( 'NONE', *, *, #2728, .F. ) ;
#4064 = DIRECTION ( 'NONE',  ( -0.000000000000000000, -1.000000000000000000, -0.000000000000000000 ) ) ;
#4065 = VERTEX_POINT ( 'NONE', #7034 ) ;
#4066 = DIRECTION ( 'NONE',  ( -0.000000000000000000, 1.000000000000000000, -0.000000000000000000 ) ) ;
#4067 = DIRECTION ( 'NONE',  ( 1.820952055660014662E-28, 1.000000000000000000, -6.508102468073347395E-30 ) ) ;
#4068 = EDGE_CURVE ( 'NONE', #517, #6620, #146, .T. ) ;
#4069 = CARTESIAN_POINT ( 'NONE',  ( -5.999999999999998224, 30.00000000000000000, 31.00000000000000711 ) ) ;
#4070 = ORIENTED_EDGE ( 'NONE', *, *, #3424, .F. ) ;
#4071 = CARTESIAN_POINT ( 'NONE',  ( 0.000000000000000000, 59.99999999999999289, 0.000000000000000000 ) ) ;
#4072 = ORIENTED_EDGE ( 'NONE', *, *, #4085, .F. ) ;
#4073 = CARTESIAN_POINT ( 'NONE',  ( 34.16461100076188018, 59.56421283147439283, 7.812829873186594831 ) ) ;
#4074 = VERTEX_POINT ( 'NONE', #925 ) ;
#4075 = EDGE_LOOP ( 'NONE', ( #1164, #5691, #9036, #8341 ) ) ;
#4076 = CARTESIAN_POINT ( 'NONE',  ( -11.54630107002959427, -4.206870269394932471, 37.25503203836519361 ) ) ;
#4077 = DIRECTION ( 'NONE',  ( -0.9860132971832694659, -1.788557213313974350E-28, 0.1666666666666658247 ) ) ;
#4078 = PLANE ( 'NONE',  #7462 ) ;
#4079 = ORIENTED_EDGE ( 'NONE', *, *, #5906, .T. ) ;
#4080 = CARTESIAN_POINT ( 'NONE',  ( 0.000000000000000000, 59.99999999999999289, 0.000000000000000000 ) ) ;
#4081 = ORIENTED_EDGE ( 'NONE', *, *, #5215, .T. ) ;
#4082 = ORIENTED_EDGE ( 'NONE', *, *, #2276, .T. ) ;
#4083 = CARTESIAN_POINT ( 'NONE',  ( 1.035379938102577995E-26, 54.50000000000031264, -24.09806918451526414 ) ) ;
#4084 = CARTESIAN_POINT ( 'NONE',  ( 5.423418723394456162E-28, -2.066522830327504070E-28, -26.00000000000008171 ) ) ;
#4085 = EDGE_CURVE ( 'NONE', #5016, #3264, #5614, .T. ) ;
#4086 = LINE ( 'NONE', #2581, #512 ) ;
#4087 = DIRECTION ( 'NONE',  ( -0.1666666666666658525, -3.897465909857536228E-29, -0.9860132971832695770 ) ) ;
#4088 = EDGE_CURVE ( 'NONE', #252, #7752, #784, .T. ) ;
#4089 = LINE ( 'NONE', #6344, #5214 ) ;
#4090 = ADVANCED_FACE ( 'NONE', ( #5476 ), #289, .T. ) ;
#4091 = CARTESIAN_POINT ( 'NONE',  ( -16.70299909897276081, 60.99999999999999289, 30.18708036726496857 ) ) ;
#4092 = VECTOR ( 'NONE', #2680, 1000.000000000000114 ) ;
#4093 = ORIENTED_EDGE ( 'NONE', *, *, #7940, .T. ) ;
#4094 = DIRECTION ( 'NONE',  ( -3.491481338843134539E-15, 0.000000000000000000, 1.000000000000000000 ) ) ;
#4095 = VERTEX_POINT ( 'NONE', #9314 ) ;
#4096 = CARTESIAN_POINT ( 'NONE',  ( -5.562309845534701758, 61.99999999999999289, 33.06426808735052703 ) ) ;
#4097 = EDGE_LOOP ( 'NONE', ( #1907, #8672, #4303, #5025, #3427 ) ) ;
#4098 = CARTESIAN_POINT ( 'NONE',  ( 6.000000000000001776, -15.00000000000000000, -26.32489316217636954 ) ) ;
#4099 = CARTESIAN_POINT ( 'NONE',  ( 6.000000000000007994, 30.00000000000000000, 26.32489316217636954 ) ) ;
#4100 = ORIENTED_EDGE ( 'NONE', *, *, #7951, .F. ) ;
#4101 = CARTESIAN_POINT ( 'NONE',  ( -13.22790787108309907, 4.939837902798808855, 36.68820129006189745 ) ) ;
#4102 = CARTESIAN_POINT ( 'NONE',  ( 33.06426808735054124, 61.99999999999999289, 1.062309845534581632 ) ) ;
#4103 = CARTESIAN_POINT ( 'NONE',  ( -37.08058572124223673, 61.87769929713620343, -7.610216775991024640 ) ) ;
#4104 = AXIS2_PLACEMENT_3D ( 'NONE', #6141, #3081, #2337 ) ;
#4105 = CIRCLE ( 'NONE', #7894, 13.53485947486097984 ) ;
#4106 = PRODUCT_RELATED_PRODUCT_CATEGORY ( 'part', '', ( #4115 ) ) ;
#4107 = CARTESIAN_POINT ( 'NONE',  ( 5.496802345886652397, -5.097331429848454221, 38.70186493977237063 ) ) ;
#4108 = DIRECTION ( 'NONE',  ( -0.000000000000000000, -1.000000000000000000, -0.000000000000000000 ) ) ;
#4109 = ORIENTED_EDGE ( 'NONE', *, *, #7585, .T. ) ;
#4110 = CARTESIAN_POINT ( 'NONE',  ( 4.000000000000008882, 28.99999999999997158, 29.00000000000000355 ) ) ;
#4111 = VERTEX_POINT ( 'NONE', #2530 ) ;
#4112 = CARTESIAN_POINT ( 'NONE',  ( 6.000000000000007994, -10.00000000000000533, 26.32489316217636954 ) ) ;
#4113 = ORIENTED_EDGE ( 'NONE', *, *, #8310, .T. ) ;
#4114 = CIRCLE ( 'NONE', #3148, 2.500000000000002220 ) ;
#4115 = PRODUCT ( 'Part2^MAS-312', 'Part2^MAS-312', '', ( #8895 ) ) ;
#4116 = DIRECTION ( 'NONE',  ( 0.000000000000000000, 1.000000000000000000, 0.000000000000000000 ) ) ;
#4117 = DIRECTION ( 'NONE',  ( 0.000000000000000000, 0.000000000000000000, 1.000000000000000000 ) ) ;
#4118 = CARTESIAN_POINT ( 'NONE',  ( 0.000000000000000000, 59.99999999999999289, 0.000000000000000000 ) ) ;
#4119 = CIRCLE ( 'NONE', #9628, 26.00000000000014566 ) ;
#4120 = ORIENTED_EDGE ( 'NONE', *, *, #335, .F. ) ;
#4121 = ORIENTED_EDGE ( 'NONE', *, *, #3648, .T. ) ;
#4122 = DIRECTION ( 'NONE',  ( -0.6195972517514871658, -0.000000000000000000, -0.7849198975831892522 ) ) ;
#4123 = ORIENTED_EDGE ( 'NONE', *, *, #6730, .F. ) ;
#4124 = LINE ( 'NONE', #1154, #8607 ) ;
#4125 = VERTEX_POINT ( 'NONE', #4871 ) ;
#4126 = ORIENTED_EDGE ( 'NONE', *, *, #8055, .T. ) ;
#4127 = CARTESIAN_POINT ( 'NONE',  ( -13.11784307232190372, 5.787500145060168855, 36.72779070367025156 ) ) ;
#4128 = DIRECTION ( 'NONE',  ( 0.000000000000000000, 1.000000000000000000, 0.000000000000000000 ) ) ;
#4129 = AXIS2_PLACEMENT_3D ( 'NONE', #3528, #2785, #1856 ) ;
#4130 = CARTESIAN_POINT ( 'NONE',  ( 8.673617379884035472E-16, 0.000000000000000000, 0.000000000000000000 ) ) ;
#4131 = ORIENTED_EDGE ( 'NONE', *, *, #2180, .T. ) ;
#4132 = DIRECTION ( 'NONE',  ( -1.735493991486225972E-29, 6.508102468073347395E-30, 1.000000000000000000 ) ) ;
#4133 = CARTESIAN_POINT ( 'NONE',  ( -8.216777476527294510, 41.50000000000020606, -23.61111111111111427 ) ) ;
#4134 = ORIENTED_EDGE ( 'NONE', *, *, #4576, .T. ) ;
#4135 = CARTESIAN_POINT ( 'NONE',  ( 1.030449557444946671E-26, 53.50000000000031264, -24.09806918451526414 ) ) ;
#4136 = LINE ( 'NONE', #6341, #8300 ) ;
#4137 = DIRECTION ( 'NONE',  ( -0.000000000000000000, -1.000000000000000000, -0.000000000000000000 ) ) ;
#4138 = CARTESIAN_POINT ( 'NONE',  ( 9.318419442923201951E-27, 47.50000000000033396, -26.00000000000011369 ) ) ;
#4139 = LINE ( 'NONE', #4873, #955 ) ;
#4140 = AXIS2_PLACEMENT_3D ( 'NONE', #679, #9720, #2941 ) ;
#4141 = DIRECTION ( 'NONE',  ( 0.000000000000000000, 0.000000000000000000, -1.000000000000000000 ) ) ;
#4142 = ADVANCED_FACE ( 'NONE', ( #8527 ), #1406, .F. ) ;
#4143 = ADVANCED_FACE ( 'NONE', ( #3184 ), #6196, .F. ) ;
#4144 = EDGE_LOOP ( 'NONE', ( #7901, #4905, #7166, #3259 ) ) ;
#4145 = EDGE_CURVE ( 'NONE', #8999, #6202, #4732, .T. ) ;
#4146 = FACE_OUTER_BOUND ( 'NONE', #4839, .T. ) ;
#4147 = ORIENTED_EDGE ( 'NONE', *, *, #9159, .T. ) ;
#4148 = DIRECTION ( 'NONE',  ( -0.000000000000000000, -1.000000000000000000, -0.000000000000000000 ) ) ;
#4149 = EDGE_LOOP ( 'NONE', ( #8277, #5838, #2902, #6814 ) ) ;
#4150 = CARTESIAN_POINT ( 'NONE',  ( -11.73250938807055377, -3.886762146447892086, 37.19966069614565640 ) ) ;
#4151 = AXIS2_PLACEMENT_3D ( 'NONE', #9377, #5630, #938 ) ;
#4152 = CARTESIAN_POINT ( 'NONE',  ( 8.673617379884035472E-16, 28.99999999999997158, 4.000000000000004441 ) ) ;
#4153 = CARTESIAN_POINT ( 'NONE',  ( -36.08344047792740383, 62.00000000000266454, -8.910509964045653319 ) ) ;
#4154 = EDGE_CURVE ( 'NONE', #8074, #1128, #3781, .T. ) ;
#4155 = ORIENTED_EDGE ( 'NONE', *, *, #5924, .F. ) ;
#4156 = LINE ( 'NONE', #1366, #4897 ) ;
#4157 = ADVANCED_FACE ( 'NONE', ( #5517 ), #3482, .F. ) ;
#4158 = VECTOR ( 'NONE', #1161, 1000.000000000000000 ) ;
#4159 = LINE ( 'NONE', #3356, #3559 ) ;
#4160 = VECTOR ( 'NONE', #6055, 1000.000000000000000 ) ;
#4161 = ORIENTED_EDGE ( 'NONE', *, *, #1418, .T. ) ;
#4162 = DIRECTION ( 'NONE',  ( 0.2840412887490734728, 0.000000000000000000, 0.9588120495101037921 ) ) ;
#4163 = ORIENTED_EDGE ( 'NONE', *, *, #1180, .T. ) ;
#4164 = DIRECTION ( 'NONE',  ( 0.9444444444444315412, 0.000000000000000000, -0.3286710990611267369 ) ) ;
#4165 = ORIENTED_EDGE ( 'NONE', *, *, #837, .T. ) ;
#4166 = CARTESIAN_POINT ( 'NONE',  ( -8.216777476527294510, 55.00000000000030553, -23.61111111111111427 ) ) ;
#4167 = CARTESIAN_POINT ( 'NONE',  ( 1.300000000000000044, 0.000000000000000000, 0.000000000000000000 ) ) ;
#4168 = CARTESIAN_POINT ( 'NONE',  ( 0.000000000000000000, 0.000000000000000000, 0.000000000000000000 ) ) ;
#4169 = DIRECTION ( 'NONE',  ( 0.000000000000000000, 0.000000000000000000, 1.000000000000000000 ) ) ;
#4170 = ORIENTED_EDGE ( 'NONE', *, *, #5490, .T. ) ;
#4171 = DIRECTION ( 'NONE',  ( 1.820952055660014662E-28, 1.000000000000000000, 7.038118388768679669E-30 ) ) ;
#4172 = ORIENTED_EDGE ( 'NONE', *, *, #7390, .F. ) ;
#4173 = DIRECTION ( 'NONE',  ( -0.000000000000000000, -1.000000000000000000, -0.000000000000000000 ) ) ;
#4174 = EDGE_LOOP ( 'NONE', ( #2011, #1833, #6874, #3858, #7895, #1839, #3316, #7750, #6, #7210, #240, #9293, #1690, #3321, #7267, #5504, #5486, #2470, #9189, #8823, #7772, #5270, #2050, #8670, #8940, #9434, #1706, #4842, #8990, #4954, #3480, #1423, #2650, #1298, #4093, #1150, #4698, #9453, #2769, #7424, #1852, #7239, #5957, #3606, #3671, #2331, #7618, #4286, #3125, #5157, #4696, #3784 ) ) ;
#4175 = CARTESIAN_POINT ( 'NONE',  ( -9.664726846066640675, 0.7061636768653499763, 41.54343935902185336 ) ) ;
#4176 = ADVANCED_FACE ( 'NONE', ( #382 ), #6484, .F. ) ;
#4177 = DIRECTION ( 'NONE',  ( -0.000000000000000000, -1.000000000000000000, -0.000000000000000000 ) ) ;
#4178 = CARTESIAN_POINT ( 'NONE',  ( -24.67792535850613334, 28.99999999999997158, -3.999999999999997335 ) ) ;
#4179 = CIRCLE ( 'NONE', #2574, 4.500000000000004441 ) ;
#4180 = EDGE_LOOP ( 'NONE', ( #6065, #7503, #2069, #3214 ) ) ;
#4181 = PLANE ( 'NONE',  #3944 ) ;
#4182 = PLANE ( 'NONE',  #3692 ) ;
#4183 = ORIENTED_EDGE ( 'NONE', *, *, #6122, .T. ) ;
#4184 = CARTESIAN_POINT ( 'NONE',  ( 12.20000000000000107, 1.971681346627238735E-16, -1.610000000000000098 ) ) ;
#4185 = CARTESIAN_POINT ( 'NONE',  ( -29.00000000000000355, 0.000000000000000000, -0.000000000000000000 ) ) ;
#4186 = FACE_BOUND ( 'NONE', #9597, .T. ) ;
#4187 = AXIS2_PLACEMENT_3D ( 'NONE', #1466, #6644, #1623 ) ;
#4188 = CARTESIAN_POINT ( 'NONE',  ( 0.000000000000000000, 0.000000000000000000, 0.000000000000000000 ) ) ;
#4189 = DIRECTION ( 'NONE',  ( -0.000000000000000000, 1.000000000000000000, -0.000000000000000000 ) ) ;
#4190 = VECTOR ( 'NONE', #6166, 1000.000000000000000 ) ;
#4191 = COLOUR_RGB ( '',0.7921568627450980005, 0.8196078431372548767, 0.9333333333333333481 ) ;
#4192 = ADVANCED_FACE ( 'NONE', ( #8125 ), #2636, .F. ) ;
#4193 = EDGE_LOOP ( 'NONE', ( #6123, #804, #4601, #2502 ) ) ;
#4194 = DIRECTION ( 'NONE',  ( 0.000000000000000000, 1.000000000000000000, 0.000000000000000000 ) ) ;
#4195 = CARTESIAN_POINT ( 'NONE',  ( 5.562309845534932684, 61.99999999999999289, -28.56426808735048439 ) ) ;
#4196 = EDGE_LOOP ( 'NONE', ( #4654, #766 ) ) ;
#4197 = DIRECTION ( 'NONE',  ( 0.3286710990610922090, 6.289316826390952918E-29, 0.9444444444444435316 ) ) ;
#4198 = FILL_AREA_STYLE ('',( #6447 ) ) ;
#4199 = CIRCLE ( 'NONE', #1031, 1.249999999999999778 ) ;
#4200 = CIRCLE ( 'NONE', #9710, 2.500000000000002220 ) ;
#4201 = CARTESIAN_POINT ( 'NONE',  ( -8.258691924487683522, 15.13224157323768182, 38.13012333692111611 ) ) ;
#4202 = AXIS2_PLACEMENT_3D ( 'NONE', #6733, #2884, #6682 ) ;
#4203 = AXIS2_PLACEMENT_3D ( 'NONE', #9004, #662, #1302 ) ;
#4204 = EDGE_CURVE ( 'NONE', #4449, #6584, #4236, .T. ) ;
#4205 = DIRECTION ( 'NONE',  ( 0.000000000000000000, 0.000000000000000000, -1.000000000000000000 ) ) ;
#4206 = AXIS2_PLACEMENT_3D ( 'NONE', #7617, #2265, #1542 ) ;
#4207 = VECTOR ( 'NONE', #1436, 1000.000000000000000 ) ;
#4208 = CARTESIAN_POINT ( 'NONE',  ( 0.000000000000000000, -15.00000000000000000, 0.000000000000000000 ) ) ;
#4209 = ORIENTED_EDGE ( 'NONE', *, *, #9537, .T. ) ;
#4210 = CARTESIAN_POINT ( 'NONE',  ( -29.82695610816121956, 39.99999999999999289, 23.54469556655648432 ) ) ;
#4211 = CARTESIAN_POINT ( 'NONE',  ( -1.783504999752484332, -15.00000000000000000, 30.27207878768652805 ) ) ;
#4212 = EDGE_LOOP ( 'NONE', ( #1986, #7139 ) ) ;
#4213 = EDGE_CURVE ( 'NONE', #9687, #9170, #1574, .T. ) ;
#4214 = VECTOR ( 'NONE', #4895, 1000.000000000000000 ) ;
#4215 = EDGE_CURVE ( 'NONE', #8266, #1456, #6291, .T. ) ;
#4216 =( BOUNDED_SURFACE ( )  B_SPLINE_SURFACE ( 3, 2, ( 
 ( #2060, #3602, #2013 ),
 ( #6602, #6414, #9624 ),
 ( #2850, #2705, #4401 ),
 ( #5141, #4995, #5036 ),
 ( #458, #9441, #8150 ),
 ( #4301, #1921, #1971 ),
 ( #5086, #6511, #5783 ),
 ( #7957, #2803, #5682 ),
 ( #3454, #8047, #8097 ),
 ( #5728, #8700, #7253 ),
 ( #2104, #409, #1192 ),
 ( #4211, #4253, #7208 ),
 ( #6456, #9483, #5865 ),
 ( #8888, #7305, #503 ),
 ( #1331, #1287, #6563 ),
 ( #8005, #1240, #3500 ),
 ( #9586, #5822, #9531 ),
 ( #2758, #556, #3555 ),
 ( #4357, #2154, #9673 ),
 ( #2895, #843, #3044 ),
 ( #2246, #5385, #2951 ),
 ( #1427, #4448, #5185 ),
 ( #6744, #9138, #7559 ),
 ( #3851, #113, #5279 ),
 ( #4599, #789, #5 ),
 ( #6848, #693, #54 ),
 ( #8297, #741, #6004 ),
 ( #7605, #3096, #5335 ),
 ( #4547, #6110, #2306 ),
 ( #1526, #3800, #6798 ),
 ( #8343, #6056, #9091 ),
 ( #1580, #7453, #6647 ),
 ( #3646, #2353, #8942 ),
 ( #8394, #1626, #3750 ),
 ( #2996, #8193, #7408 ),
 ( #642, #3697, #9038 ),
 ( #6699, #5959, #5915 ),
 ( #4495, #9728, #8985 ) ),
 .UNSPECIFIED., .F., .F., .F. ) 
 B_SPLINE_SURFACE_WITH_KNOTS ( ( 4, 2, 2, 2, 2, 2, 2, 2, 2, 2, 2, 2, 2, 2, 2, 2, 2, 2, 4 ),
 ( 3, 3 ),
 ( 1.795438797635995343E-16, 0.002181780987149469723, 0.003272671480724114595, 0.004363561974298759902, 0.005454452467873405208, 0.006545342961448049647, 0.007636233455022694086, 0.008181678701810017607, 0.008727123948597339392, 0.008999846571991000285, 0.009272569195384661178, 0.009818014442171984699, 0.01036345968895930822, 0.01090890493574663000, 0.01199979542932127358, 0.01309068592289591888, 0.01418157641647056419, 0.01527246691004520776, 0.01745424789719449837 ),
 ( 0.000000000000000000, 1.000000000000000000 ),
 .UNSPECIFIED. ) 
 GEOMETRIC_REPRESENTATION_ITEM ( )  RATIONAL_B_SPLINE_SURFACE ( (
 ( 1.000000000000000000, 0.7071067811865473507, 1.000000000000000000),
 ( 1.000000000000000000, 0.7161513553615299621, 1.000000000000000000),
 ( 1.000000000000000000, 0.7261151885358542168, 1.000000000000000000),
 ( 1.000000000000000000, 0.7427909353351239696, 1.000000000000000000),
 ( 1.000000000000000000, 0.7486383365456040773, 1.000000000000000000),
 ( 1.000000000000000000, 0.7609590083029650343, 1.000000000000000000),
 ( 1.000000000000000000, 0.7674338186474088941, 1.000000000000000000),
 ( 1.000000000000000000, 0.7810218732661525776, 1.000000000000000000),
 ( 1.000000000000000000, 0.7881405391415673423, 1.000000000000000000),
 ( 1.000000000000000000, 0.8029038133575651104, 1.000000000000000000),
 ( 1.000000000000000000, 0.8105722495354327206, 1.000000000000000000),
 ( 1.000000000000000000, 0.8258428283520197200, 1.000000000000000000),
 ( 1.000000000000000000, 0.8335350131668984863, 1.000000000000000000),
 ( 1.000000000000000000, 0.8428590422713853059, 1.000000000000000000),
 ( 1.000000000000000000, 0.8455698979328197806, 1.000000000000000000),
 ( 1.000000000000000000, 0.8494339551369524122, 1.000000000000000000),
 ( 1.000000000000000000, 0.8505582715026442919, 1.000000000000000000),
 ( 1.000000000000000000, 0.8506061670060169888, 1.000000000000000000),
 ( 1.000000000000000000, 0.8503513266545774663, 1.000000000000000000),
 ( 1.000000000000000000, 0.8493382604359895893, 1.000000000000000000),
 ( 1.000000000000000000, 0.8485833736532394367, 1.000000000000000000),
 ( 1.000000000000000000, 0.8457164237044830779, 1.000000000000000000),
 ( 1.000000000000000000, 0.8430121088779416461, 1.000000000000000000),
 ( 1.000000000000000000, 0.8368088722261513013, 1.000000000000000000),
 ( 1.000000000000000000, 0.8333129582802408786, 1.000000000000000000),
 ( 1.000000000000000000, 0.8260259447890396789, 1.000000000000000000),
 ( 1.000000000000000000, 0.8222304458373403957, 1.000000000000000000),
 ( 1.000000000000000000, 0.8107652166501773117, 1.000000000000000000),
 ( 1.000000000000000000, 0.8030801492908825612, 1.000000000000000000),
 ( 1.000000000000000000, 0.7882884757859640601, 1.000000000000000000),
 ( 1.000000000000000000, 0.7811556660049406853, 1.000000000000000000),
 ( 1.000000000000000000, 0.7675411181467285404, 1.000000000000000000),
 ( 1.000000000000000000, 0.7610538784716394112, 1.000000000000000000),
 ( 1.000000000000000000, 0.7487101099141471039, 1.000000000000000000),
 ( 1.000000000000000000, 0.7428520250537596903, 1.000000000000000000),
 ( 1.000000000000000000, 0.7261465437174193793, 1.000000000000000000),
 ( 1.000000000000000000, 0.7161659583961312858, 1.000000000000000000),
 ( 1.000000000000000000, 0.7071067811865477948, 1.000000000000000000) ) ) 
 REPRESENTATION_ITEM ( '' )  SURFACE ( )  );
#4217 = ADVANCED_FACE ( 'NONE', ( #483 ), #6393, .F. ) ;
#4218 = DIRECTION ( 'NONE',  ( 0.000000000000000000, 0.7071067811865376918, -0.7071067811865573427 ) ) ;
#4219 = CARTESIAN_POINT ( 'NONE',  ( 2.400000000000000799, 2.449293598294705921E-16, -1.999999999999999556 ) ) ;
#4220 = CARTESIAN_POINT ( 'NONE',  ( -33.06426808735054124, 60.99999999999999289, -5.562309845534581854 ) ) ;
#4221 = ORIENTED_EDGE ( 'NONE', *, *, #5936, .F. ) ;
#4222 = PLANE ( 'NONE',  #4823 ) ;
#4223 = ORIENTED_EDGE ( 'NONE', *, *, #6311, .F. ) ;
#4224 = DIRECTION ( 'NONE',  ( -1.000000000000000000, -0.000000000000000000, -0.000000000000000000 ) ) ;
#4225 = ORIENTED_EDGE ( 'NONE', *, *, #6237, .F. ) ;
#4226 = AXIS2_PLACEMENT_3D ( 'NONE', #8824, #2047, #1273 ) ;
#4227 = ORIENTED_EDGE ( 'NONE', *, *, #5172, .T. ) ;
#4228 = CARTESIAN_POINT ( 'NONE',  ( -7.530772855371751895, -3.328027317286678777, 38.39592399675708378 ) ) ;
#4229 = DIRECTION ( 'NONE',  ( 0.000000000000000000, 0.000000000000000000, 1.000000000000000000 ) ) ;
#4230 = DIRECTION ( 'NONE',  ( -0.3286710990610922090, -6.289316826390952918E-29, -0.9444444444444435316 ) ) ;
#4231 = VERTEX_POINT ( 'NONE', #5663 ) ;
#4232 = DIRECTION ( 'NONE',  ( -0.7849198975831892522, 0.000000000000000000, 0.6195972517514871658 ) ) ;
#4233 = ORIENTED_EDGE ( 'NONE', *, *, #3957, .F. ) ;
#4234 = VERTEX_POINT ( 'NONE', #5065 ) ;
#4235 = CARTESIAN_POINT ( 'NONE',  ( 0.000000000000000000, 59.99999999999999289, 0.000000000000000000 ) ) ;
#4236 = LINE ( 'NONE', #4185, #9154 ) ;
#4237 = CARTESIAN_POINT ( 'NONE',  ( 12.77996869406904068, 7.481990194735835153, 36.84712280227347492 ) ) ;
#4238 = DIRECTION ( 'NONE',  ( -0.000000000000000000, 1.000000000000000000, -0.000000000000000000 ) ) ;
#4239 = LINE ( 'NONE', #486, #6223 ) ;
#4240 = ORIENTED_EDGE ( 'NONE', *, *, #4579, .T. ) ;
#4241 = FACE_BOUND ( 'NONE', #1294, .T. ) ;
#4242 =( REPRESENTATION_RELATIONSHIP ('NONE','NONE', #5841, #490 ) REPRESENTATION_RELATIONSHIP_WITH_TRANSFORMATION ( #7664 )SHAPE_REPRESENTATION_RELATIONSHIP( ) );
#4243 = CARTESIAN_POINT ( 'NONE',  ( 9.916385959428817287, 4.627893224472521716, 41.40953687719313336 ) ) ;
#4244 = ORIENTED_EDGE ( 'NONE', *, *, #5215, .F. ) ;
#4245 = DIRECTION ( 'NONE',  ( -1.000000000000000000, 0.000000000000000000, 0.000000000000000000 ) ) ;
#4246 = DIRECTION ( 'NONE',  ( -0.000000000000000000, -1.000000000000000000, -0.000000000000000000 ) ) ;
#4247 = LINE ( 'NONE', #5674, #7644 ) ;
#4248 = CARTESIAN_POINT ( 'NONE',  ( 3.538670939391739712, -8.984539127871803643, 39.30863205750186751 ) ) ;
#4249 = EDGE_CURVE ( 'NONE', #4378, #9481, #3519, .T. ) ;
#4250 = DIRECTION ( 'NONE',  ( -2.168404344971006649E-16, 0.000000000000000000, -1.000000000000000000 ) ) ;
#4251 = EDGE_LOOP ( 'NONE', ( #7206, #675, #6435, #5574, #3442, #7969 ) ) ;
#4252 = DIRECTION ( 'NONE',  ( -0.000000000000000000, 1.000000000000000000, -0.000000000000000000 ) ) ;
#4253 = CARTESIAN_POINT ( 'NONE',  ( -3.866809454646866318, -15.00000000000031442, 36.77917012741243497 ) ) ;
#4254 = VERTEX_POINT ( 'NONE', #3581 ) ;
#4255 = LINE ( 'NONE', #6459, #5554 ) ;
#4256 = VECTOR ( 'NONE', #3933, 1000.000000000000000 ) ;
#4257 = CIRCLE ( 'NONE', #3458, 1.610000000000000098 ) ;
#4258 = CARTESIAN_POINT ( 'NONE',  ( 16.29881421347312909, 60.99999999999999289, -2.568784777805685593 ) ) ;
#4259 = CARTESIAN_POINT ( 'NONE',  ( 8.371299763093835722, 8.807943335447152577, 38.23376413749986114 ) ) ;
#4260 = EDGE_CURVE ( 'NONE', #2949, #9099, #534, .T. ) ;
#4261 = EDGE_CURVE ( 'NONE', #7439, #64, #7246, .T. ) ;
#4262 = DIRECTION ( 'NONE',  ( 1.000000000000000000, 0.000000000000000000, 0.000000000000000000 ) ) ;
#4263 = ORIENTED_EDGE ( 'NONE', *, *, #2084, .F. ) ;
#4264 = DIRECTION ( 'NONE',  ( 0.000000000000000000, 0.000000000000000000, 1.000000000000000000 ) ) ;
#4265 = EDGE_CURVE ( 'NONE', #4910, #1089, #4105, .T. ) ;
#4266 = ORIENTED_EDGE ( 'NONE', *, *, #5170, .F. ) ;
#4267 = DIRECTION ( 'NONE',  ( -1.820952055660014662E-28, -1.000000000000000000, -7.038118388768679669E-30 ) ) ;
#4268 = ORIENTED_EDGE ( 'NONE', *, *, #7755, .F. ) ;
#4269 = CIRCLE ( 'NONE', #5378, 2.499999999999998668 ) ;
#4270 = VERTEX_POINT ( 'NONE', #1314 ) ;
#4271 = CARTESIAN_POINT ( 'NONE',  ( -3.570894301289286421, 12.65974171353586719, 38.88496779480359322 ) ) ;
#4272 = DIRECTION ( 'NONE',  ( 1.820952055660014662E-28, 1.000000000000000000, -6.508102468073347395E-30 ) ) ;
#4273 = CARTESIAN_POINT ( 'NONE',  ( -5.999999999999998224, 28.28385863652524179, 30.12488991936162464 ) ) ;
#4274 = AXIS2_PLACEMENT_3D ( 'NONE', #927, #6838, #8432 ) ;
#4275 = EDGE_CURVE ( 'NONE', #742, #5194, #5018, .T. ) ;
#4276 = ORIENTED_EDGE ( 'NONE', *, *, #3630, .F. ) ;
#4277 = DIRECTION ( 'NONE',  ( 0.000000000000000000, 0.000000000000000000, 1.000000000000000000 ) ) ;
#4278 = EDGE_CURVE ( 'NONE', #4551, #8213, #2981, .T. ) ;
#4279 = LINE ( 'NONE', #2036, #6991 ) ;
#4280 = EDGE_LOOP ( 'NONE', ( #5747, #2102, #6895, #7703 ) ) ;
#4281 = DIRECTION ( 'NONE',  ( 0.000000000000000000, 0.000000000000000000, 1.000000000000000000 ) ) ;
#4282 = DIRECTION ( 'NONE',  ( 0.000000000000000000, 0.000000000000000000, -1.000000000000000000 ) ) ;
#4283 = FACE_OUTER_BOUND ( 'NONE', #9401, .T. ) ;
#4284 = LINE ( 'NONE', #8127, #7100 ) ;
#4285 = PLANE ( 'NONE',  #1340 ) ;
#4286 = ORIENTED_EDGE ( 'NONE', *, *, #1715, .T. ) ;
#4287 = DIRECTION ( 'NONE',  ( 0.000000000000000000, 1.000000000000000000, 0.000000000000000000 ) ) ;
#4288 = CARTESIAN_POINT ( 'NONE',  ( 9.219811829770575476E-27, 46.00000000000018474, -24.09806918451533875 ) ) ;
#4289 = ORIENTED_EDGE ( 'NONE', *, *, #5485, .T. ) ;
#4290 = FACE_OUTER_BOUND ( 'NONE', #1941, .T. ) ;
#4291 = CARTESIAN_POINT ( 'NONE',  ( 8.677469957431129860E-27, 43.00000000000019895, -25.00000000000000000 ) ) ;
#4292 = CARTESIAN_POINT ( 'NONE',  ( 4.653657836759942730E-15, 0.000000000000000000, 38.00000000000000711 ) ) ;
#4293 = ADVANCED_FACE ( 'NONE', ( #8771 ), #2039, .T. ) ;
#4294 = CARTESIAN_POINT ( 'NONE',  ( 0.000000000000000000, 58.99999999999999289, -38.00000000000000711 ) ) ;
#4295 = VECTOR ( 'NONE', #8153, 1000.000000000000000 ) ;
#4296 = APPLICATION_CONTEXT ( 'automotive_design' ) ;
#4297 = DIRECTION ( 'NONE',  ( -1.000000000000000000, 0.000000000000000000, 1.084202172485503448E-16 ) ) ;
#4298 = DIRECTION ( 'NONE',  ( 0.000000000000000000, 1.000000000000000000, 0.000000000000000000 ) ) ;
#4299 = ORIENTED_EDGE ( 'NONE', *, *, #3277, .F. ) ;
#4300 = LINE ( 'NONE', #599, #1188 ) ;
#4301 = CARTESIAN_POINT ( 'NONE',  ( -4.822208557843039145, -15.00000000000000000, 29.05578429771093951 ) ) ;
#4302 = VECTOR ( 'NONE', #5530, 1000.000000000000000 ) ;
#4303 = ORIENTED_EDGE ( 'NONE', *, *, #8261, .T. ) ;
#4304 = DIRECTION ( 'NONE',  ( 0.000000000000000000, 0.000000000000000000, 1.000000000000000000 ) ) ;
#4305 = CARTESIAN_POINT ( 'NONE',  ( 2.400000000000000799, 0.000000000000000000, 1.999999999999999556 ) ) ;
#4306 = AXIS2_PLACEMENT_3D ( 'NONE', #980, #9432, #1131 ) ;
#4307 = CARTESIAN_POINT ( 'NONE',  ( 2.211399979663802196, 18.09417943208245205, 38.93963529505569454 ) ) ;
#4308 = EDGE_CURVE ( 'NONE', #6509, #8688, #5365, .T. ) ;
#4309 = ORIENTED_EDGE ( 'NONE', *, *, #6122, .F. ) ;
#4310 = CARTESIAN_POINT ( 'NONE',  ( 0.000000000000000000, 1.000000000000014655, 17.99999999999999645 ) ) ;
#4311 = ORIENTED_EDGE ( 'NONE', *, *, #5070, .F. ) ;
#4312 = LINE ( 'NONE', #6520, #9073 ) ;
#4313 = ORIENTED_EDGE ( 'NONE', *, *, #5344, .F. ) ;
#4314 = LINE ( 'NONE', #7316, #7355 ) ;
#4315 = ORIENTED_EDGE ( 'NONE', *, *, #8557, .F. ) ;
#4316 = CARTESIAN_POINT ( 'NONE',  ( -5.282492592870707604, 11.79197944368125839, 43.28262095644331708 ) ) ;
#4317 = AXIS2_PLACEMENT_3D ( 'NONE', #3871, #6870, #4117 ) ;
#4318 = PLANE ( 'NONE',  #4827 ) ;
#4319 = EDGE_CURVE ( 'NONE', #2789, #8766, #320, .T. ) ;
#4320 = CARTESIAN_POINT ( 'NONE',  ( 12.20000000000000107, 0.000000000000000000, 1.610000000000000098 ) ) ;
#4321 = ADVANCED_FACE ( 'NONE', ( #4327 ), #7333, .F. ) ;
#4322 = ORIENTED_EDGE ( 'NONE', *, *, #6251, .T. ) ;
#4323 = DIRECTION ( 'NONE',  ( -1.820952055660014662E-28, -1.000000000000000000, -7.038118388768679669E-30 ) ) ;
#4324 = DIRECTION ( 'NONE',  ( -0.000000000000000000, 0.5000000000000000000, 0.8660254037844385966 ) ) ;
#4325 = ORIENTED_EDGE ( 'NONE', *, *, #991, .F. ) ;
#4326 = DIRECTION ( 'NONE',  ( -0.000000000000000000, -1.000000000000000000, -0.000000000000000000 ) ) ;
#4327 = FACE_OUTER_BOUND ( 'NONE', #3097, .T. ) ;
#4328 = EDGE_CURVE ( 'NONE', #7752, #137, #7084, .T. ) ;
#4329 = FACE_OUTER_BOUND ( 'NONE', #2123, .T. ) ;
#4330 = CARTESIAN_POINT ( 'NONE',  ( 4.714890176717311093E-15, 61.99999999999999289, 37.00000000000001421 ) ) ;
#4331 = EDGE_CURVE ( 'NONE', #1750, #1639, #6607, .T. ) ;
#4332 = DIRECTION ( 'NONE',  ( 0.000000000000000000, 0.000000000000000000, 1.000000000000000000 ) ) ;
#4333 = ADVANCED_FACE ( 'NONE', ( #4572 ), #7537, .F. ) ;
#4334 = CIRCLE ( 'NONE', #5746, 5.000000000000001776 ) ;
#4335 = EDGE_CURVE ( 'NONE', #2857, #5882, #7479, .T. ) ;
#4336 = B_SPLINE_CURVE_WITH_KNOTS ( 'NONE', 3,
 ( #7044, #4516, #1821, #2268, #6815, #2322, #8587, #2211, #9743, #301, #2966, #1034, #9003, #131, #3296, #4616, #7473, #7572, #8358, #1545, #6305, #859, #2544, #72, #8315, #3867 ),
 .UNSPECIFIED., .F., .F.,
 ( 4, 2, 2, 2, 2, 2, 2, 2, 2, 2, 2, 2, 4 ),
 ( 0.03173335151219601469, 0.03272663708407346633, 0.03371992265595091104, 0.03570649379970581433, 0.03669977937158326597, 0.03769306494346071068, 0.03967963608721561397, 0.04067292165909306562, 0.04166620723097052420, 0.04365277837472542055, 0.04563934951848032384, 0.04663263509035776855, 0.04762592066223522019 ),
 .UNSPECIFIED. ) ;
#4337 = DIRECTION ( 'NONE',  ( 0.000000000000000000, -1.000000000000000000, 0.000000000000000000 ) ) ;
#4338 = TOROIDAL_SURFACE ( 'NONE', #8272, 29.00000000000001776, 10.00000000000000000 ) ;
#4339 = ORIENTED_EDGE ( 'NONE', *, *, #5211, .F. ) ;
#4340 = AXIS2_PLACEMENT_3D ( 'NONE', #1523, #9725, #50 ) ;
#4341 = FACE_OUTER_BOUND ( 'NONE', #8963, .T. ) ;
#4342 = CARTESIAN_POINT ( 'NONE',  ( 2.649740526188390621, 12.96017046470857359, 43.83099598276683651 ) ) ;
#4343 = ORIENTED_EDGE ( 'NONE', *, *, #6720, .T. ) ;
#4344 = PLANE ( 'NONE',  #1916 ) ;
#4345 = FACE_OUTER_BOUND ( 'NONE', #6126, .T. ) ;
#4346 = CARTESIAN_POINT ( 'NONE',  ( 3.885274725274726393, -8.673617379884035472E-16, 0.000000000000000000 ) ) ;
#4347 = CIRCLE ( 'NONE', #2434, 26.00000000000011369 ) ;
#4348 = AXIS2_PLACEMENT_3D ( 'NONE', #2978, #8271, #9608 ) ;
#4349 = VECTOR ( 'NONE', #4854, 1000.000000000000000 ) ;
#4350 = FACE_BOUND ( 'NONE', #4591, .T. ) ;
#4351 = AXIS2_PLACEMENT_3D ( 'NONE', #7418, #9636, #655 ) ;
#4352 = CARTESIAN_POINT ( 'NONE',  ( -8.216777476527294510, 43.00000000000019895, -23.61111111111111427 ) ) ;
#4353 = VECTOR ( 'NONE', #6427, 1000.000000000000000 ) ;
#4354 = COLOUR_RGB ( '',0.7921568627450980005, 0.8196078431372548767, 0.9333333333333333481 ) ;
#4355 = ORIENTED_EDGE ( 'NONE', *, *, #6309, .T. ) ;
#4356 = LINE ( 'NONE', #3499, #1655 ) ;
#4357 = CARTESIAN_POINT ( 'NONE',  ( 0.1750943534869517371, -15.00000000000000178, 30.57953220782976800 ) ) ;
#4358 = ORIENTED_EDGE ( 'NONE', *, *, #749, .F. ) ;
#4359 = CARTESIAN_POINT ( 'NONE',  ( 24.67792535850613334, 30.00000000000000000, 4.000000000000000888 ) ) ;
#4360 = VECTOR ( 'NONE', #8163, 1000.000000000000000 ) ;
#4361 = CIRCLE ( 'NONE', #109, 1.249999999999999778 ) ;
#4362 = CARTESIAN_POINT ( 'NONE',  ( 0.000000000000000000, 30.00000000000000000, 0.000000000000000000 ) ) ;
#4363 = ORIENTED_EDGE ( 'NONE', *, *, #937, .T. ) ;
#4364 = CARTESIAN_POINT ( 'NONE',  ( 0.6754392200130907575, 13.27748550001718897, 43.99110106382870811 ) ) ;
#4365 = CARTESIAN_POINT ( 'NONE',  ( 0.000000000000000000, 0.000000000000000000, 0.000000000000000000 ) ) ;
#4366 = VERTEX_POINT ( 'NONE', #6032 ) ;
#4367 = FACE_OUTER_BOUND ( 'NONE', #9503, .T. ) ;
#4368 = AXIS2_PLACEMENT_3D ( 'NONE', #5718, #1325, #451 ) ;
#4369 = DIRECTION ( 'NONE',  ( 0.000000000000000000, 1.000000000000000000, 0.000000000000000000 ) ) ;
#4370 = ORIENTED_EDGE ( 'NONE', *, *, #7816, .F. ) ;
#4371 = FACE_OUTER_BOUND ( 'NONE', #3877, .T. ) ;
#4372 = VERTEX_POINT ( 'NONE', #4527 ) ;
#4373 = CARTESIAN_POINT ( 'NONE',  ( -4.125509516341439031, 12.41002393623410605, 43.56504187369129255 ) ) ;
#4374 = DIRECTION ( 'NONE',  ( -1.000000000000000000, 0.000000000000000000, 0.000000000000000000 ) ) ;
#4375 = EDGE_CURVE ( 'NONE', #6509, #1980, #1361, .T. ) ;
#4376 = CARTESIAN_POINT ( 'NONE',  ( 1.042775509089024980E-26, 52.00000000000031974, -26.00000000000006395 ) ) ;
#4377 = CIRCLE ( 'NONE', #8569, 4.999999999999999112 ) ;
#4378 = VERTEX_POINT ( 'NONE', #767 ) ;
#4379 = CARTESIAN_POINT ( 'NONE',  ( 26.32489316217636954, 30.00000000000000000, -6.000000000000006217 ) ) ;
#4380 = ORIENTED_EDGE ( 'NONE', *, *, #2549, .T. ) ;
#4381 = DIRECTION ( 'NONE',  ( -1.820952055660014662E-28, -1.000000000000000000, -7.038118388768679669E-30 ) ) ;
#4382 = DIRECTION ( 'NONE',  ( 1.000000000000000000, -0.000000000000000000, 1.047444401652940795E-14 ) ) ;
#4383 =( NAMED_UNIT ( * ) PLANE_ANGLE_UNIT ( ) SI_UNIT ( $, .RADIAN. ) );
#4384 = CARTESIAN_POINT ( 'NONE',  ( 1.138917931912835794E-26, 58.00000000000029132, -25.00000000000000000 ) ) ;
#4385 = CARTESIAN_POINT ( 'NONE',  ( -3.999999999999998224, 30.00000000000000000, 29.00000000000000355 ) ) ;
#4386 = CARTESIAN_POINT ( 'NONE',  ( 0.000000000000000000, 52.29648987751954792, 0.000000000000000000 ) ) ;
#4387 = EDGE_CURVE ( 'NONE', #1101, #9714, #4888, .T. ) ;
#4388 = EDGE_CURVE ( 'NONE', #3204, #294, #3730, .T. ) ;
#4389 = ORIENTED_EDGE ( 'NONE', *, *, #2832, .T. ) ;
#4390 = DIRECTION ( 'NONE',  ( 0.000000000000000000, 0.000000000000000000, 1.000000000000000000 ) ) ;
#4391 = FACE_OUTER_BOUND ( 'NONE', #9749, .T. ) ;
#4392 = CARTESIAN_POINT ( 'NONE',  ( 5.423418723394456162E-28, -2.066522830327504070E-28, -26.00000000000014566 ) ) ;
#4393 = EDGE_CURVE ( 'NONE', #5506, #7120, #7299, .T. ) ;
#4394 = LINE ( 'NONE', #7396, #3357 ) ;
#4395 = DIRECTION ( 'NONE',  ( -0.1666666666666658525, -3.897465909857536228E-29, -0.9860132971832695770 ) ) ;
#4396 = PLANE ( 'NONE',  #8116 ) ;
#4397 = DIRECTION ( 'NONE',  ( -1.000000000000000000, -0.000000000000000000, -0.000000000000000000 ) ) ;
#4398 = CARTESIAN_POINT ( 'NONE',  ( 0.000000000000000000, 60.99999999999999289, 0.000000000000000000 ) ) ;
#4399 = EDGE_LOOP ( 'NONE', ( #949, #6609, #2826, #5162 ) ) ;
#4400 = LINE ( 'NONE', #3453, #7463 ) ;
#4401 = CARTESIAN_POINT ( 'NONE',  ( -10.24028423210522476, -5.542393513087790602, 37.65233335542363591 ) ) ;
#4402 = ORIENTED_EDGE ( 'NONE', *, *, #6066, .F. ) ;
#4403 = DIRECTION ( 'NONE',  ( 0.9860132971832693549, 1.788557213313974126E-28, -0.1666666666666657970 ) ) ;
#4404 = CARTESIAN_POINT ( 'NONE',  ( 0.000000000000000000, 0.7216878364870328300, -1.250000000000000000 ) ) ;
#4405 = ORIENTED_EDGE ( 'NONE', *, *, #8307, .F. ) ;
#4406 = CARTESIAN_POINT ( 'NONE',  ( 11.52123655141487113, 10.79705879502866139, 37.25999260019175097 ) ) ;
#4407 = ORIENTED_EDGE ( 'NONE', *, *, #3429, .T. ) ;
#4408 = DIRECTION ( 'NONE',  ( -0.000000000000000000, 1.000000000000000000, -0.000000000000000000 ) ) ;
#4409 = CARTESIAN_POINT ( 'NONE',  ( 9.762153702110021092E-27, 50.50000000000031974, -25.00000000000000000 ) ) ;
#4410 = ORIENTED_EDGE ( 'NONE', *, *, #5825, .F. ) ;
#4411 = CARTESIAN_POINT ( 'NONE',  ( -8.545448575588423523, -1.752403656397945903E-27, -24.55555555555572766 ) ) ;
#4412 = EDGE_LOOP ( 'NONE', ( #8709, #7700, #5963, #4443 ) ) ;
#4413 = CARTESIAN_POINT ( 'NONE',  ( -1.720948704681326991, 18.17687923655758553, 38.96445573820884078 ) ) ;
#4414 = AXIS2_PLACEMENT_3D ( 'NONE', #6628, #3626, #8217 ) ;
#4415 = EDGE_CURVE ( 'NONE', #179, #1752, #6138, .T. ) ;
#4416 = DIRECTION ( 'NONE',  ( -0.000000000000000000, -1.000000000000000000, -0.000000000000000000 ) ) ;
#4417 = LINE ( 'NONE', #8115, #7937 ) ;
#4418 = AXIS2_PLACEMENT_3D ( 'NONE', #8379, #4634, #6882 ) ;
#4419 = AXIS2_PLACEMENT_3D ( 'NONE', #9713, #8135, #3735 ) ;
#4420 = ORIENTED_EDGE ( 'NONE', *, *, #6549, .F. ) ;
#4421 = FACE_OUTER_BOUND ( 'NONE', #8513, .T. ) ;
#4422 = ORIENTED_EDGE ( 'NONE', *, *, #9701, .F. ) ;
#4423 = DIRECTION ( 'NONE',  ( 0.000000000000000000, 0.7071067811865451302, 0.7071067811865500152 ) ) ;
#4424 = CARTESIAN_POINT ( 'NONE',  ( 0.000000000000000000, 39.99999999999999289, 0.000000000000000000 ) ) ;
#4425 = DIRECTION ( 'NONE',  ( -0.000000000000000000, -1.000000000000000000, -0.000000000000000000 ) ) ;
#4426 = VECTOR ( 'NONE', #99, 1000.000000000000114 ) ;
#4427 = CARTESIAN_POINT ( 'NONE',  ( 4.665243217607707216, 29.66524321760768856, 25.23917843705063646 ) ) ;
#4428 = AXIS2_PLACEMENT_3D ( 'NONE', #79, #9061, #4623 ) ;
#4429 = ORIENTED_EDGE ( 'NONE', *, *, #8307, .T. ) ;
#4430 = EDGE_CURVE ( 'NONE', #7824, #2152, #6133, .T. ) ;
#4431 = CARTESIAN_POINT ( 'NONE',  ( -30.00000000000000711, 30.00000000000000000, 0.000000000000000000 ) ) ;
#4432 = DIRECTION ( 'NONE',  ( 0.000000000000000000, -0.000000000000000000, 1.000000000000000000 ) ) ;
#4433 = VECTOR ( 'NONE', #6044, 1000.000000000000000 ) ;
#4434 = DIRECTION ( 'NONE',  ( -0.000000000000000000, -1.000000000000000000, -0.000000000000000000 ) ) ;
#4435 = DIRECTION ( 'NONE',  ( 0.9444444444444436426, 1.704463408222248963E-28, -0.3286710990610922645 ) ) ;
#4436 = PLANE ( 'NONE',  #653 ) ;
#4437 = CARTESIAN_POINT ( 'NONE',  ( -31.00000000000000711, 27.80235549540589801, -4.012532818320189598 ) ) ;
#4438 = EDGE_CURVE ( 'NONE', #5147, #4501, #1402, .T. ) ;
#4439 = AXIS2_PLACEMENT_3D ( 'NONE', #8169, #5888, #5163 ) ;
#4440 = ADVANCED_FACE ( 'NONE', ( #6770 ), #27, .T. ) ;
#4441 = ADVANCED_FACE ( 'NONE', ( #3675 ), #2933, .T. ) ;
#4442 = FACE_OUTER_BOUND ( 'NONE', #4019, .T. ) ;
#4443 = ORIENTED_EDGE ( 'NONE', *, *, #2844, .T. ) ;
#4444 = DIRECTION ( 'NONE',  ( 0.000000000000000000, 0.000000000000000000, 1.000000000000000000 ) ) ;
#4445 = DIRECTION ( 'NONE',  ( -1.000000000000000000, 0.000000000000000000, 0.000000000000000000 ) ) ;
#4446 = ORIENTED_EDGE ( 'NONE', *, *, #9520, .F. ) ;
#4447 = CARTESIAN_POINT ( 'NONE',  ( 0.000000000000000000, -10.00000000000000533, 0.000000000000000000 ) ) ;
#4448 = CARTESIAN_POINT ( 'NONE',  ( 1.689983091256852976, -15.00000000000062883, 36.76756119980281312 ) ) ;
#4449 = VERTEX_POINT ( 'NONE', #9705 ) ;
#4450 = CIRCLE ( 'NONE', #3979, 13.53485947486097984 ) ;
#4451 = EDGE_CURVE ( 'NONE', #6620, #7071, #1556, .T. ) ;
#4452 = CARTESIAN_POINT ( 'NONE',  ( 1.094544505994153880E-26, 56.50000000000029843, -25.00000000000000000 ) ) ;
#4453 = ADVANCED_BREP_SHAPE_REPRESENTATION ( '', ( #9696, #6314 ), #6474 ) ;
#4454 = DIRECTION ( 'NONE',  ( 0.000000000000000000, 1.000000000000000000, 0.000000000000000000 ) ) ;
#4455 = ORIENTED_EDGE ( 'NONE', *, *, #5775, .F. ) ;
#4456 = EDGE_CURVE ( 'NONE', #6645, #7858, #5201, .T. ) ;
#4457 = ADVANCED_FACE ( 'NONE', ( #7214 ), #3244, .F. ) ;
#4458 = TOROIDAL_SURFACE ( 'NONE', #7607, 33.00000000000000711, 5.000000000000000000 ) ;
#4459 = ORIENTED_EDGE ( 'NONE', *, *, #7023, .T. ) ;
#4460 = LINE ( 'NONE', #5242, #2605 ) ;
#4461 = ORIENTED_EDGE ( 'NONE', *, *, #2184, .F. ) ;
#4462 = CARTESIAN_POINT ( 'NONE',  ( 9.196165333680795946E-27, 50.50000000000031974, 3.170080688461390214E-28 ) ) ;
#4463 = EDGE_LOOP ( 'NONE', ( #7545, #1272, #3579, #2004 ) ) ;
#4464 = CARTESIAN_POINT ( 'NONE',  ( -5.562309845534584518, 69.99999999999998579, 30.56426808735054124 ) ) ;
#4465 = ORIENTED_EDGE ( 'NONE', *, *, #8541, .T. ) ;
#4466 = CARTESIAN_POINT ( 'NONE',  ( -2.185593797502169089, 13.07767852523060803, 38.96206052328675185 ) ) ;
#4467 = CARTESIAN_POINT ( 'NONE',  ( 1.047999611769018552E-26, 57.50000000000029843, 3.031413732465509233E-28 ) ) ;
#4468 = AXIS2_PLACEMENT_3D ( 'NONE', #5576, #1823, #3449 ) ;
#4469 = DIRECTION ( 'NONE',  ( 0.000000000000000000, 0.000000000000000000, -1.000000000000000000 ) ) ;
#4470 = EDGE_LOOP ( 'NONE', ( #3171, #8151, #1476, #4625 ) ) ;
#4471 = CARTESIAN_POINT ( 'NONE',  ( 0.000000000000000000, 61.99999999999999289, 0.000000000000000000 ) ) ;
#4472 = ORIENTED_EDGE ( 'NONE', *, *, #1950, .T. ) ;
#4473 = AXIS2_PLACEMENT_3D ( 'NONE', #9600, #7475, #714 ) ;
#4474 = EDGE_CURVE ( 'NONE', #5419, #3082, #2177, .T. ) ;
#4475 = CARTESIAN_POINT ( 'NONE',  ( -30.00000000000001066, 59.99999999999999289, -3.142333204958820777E-13 ) ) ;
#4476 = CARTESIAN_POINT ( 'NONE',  ( 33.06426808735054124, 60.99999999999999289, 5.562309845534586294 ) ) ;
#4477 = PLANE ( 'NONE',  #250 ) ;
#4478 = CYLINDRICAL_SURFACE ( 'NONE', #523, 40.00000000000000711 ) ;
#4479 = CARTESIAN_POINT ( 'NONE',  ( 5.000000000000002665, 30.00000000000000000, -25.51470164434615029 ) ) ;
#4480 = ORIENTED_EDGE ( 'NONE', *, *, #2130, .T. ) ;
#4481 = DIRECTION ( 'NONE',  ( -1.000000000000000000, -0.000000000000000000, -0.000000000000000000 ) ) ;
#4482 = DIRECTION ( 'NONE',  ( 0.000000000000000000, 0.000000000000000000, 1.000000000000000000 ) ) ;
#4483 = CARTESIAN_POINT ( 'NONE',  ( 8.237197373723128990, -15.00000000000000000, 27.80554943579302574 ) ) ;
#4484 = CARTESIAN_POINT ( 'NONE',  ( -4.999999999999998224, 30.00000000000000000, 25.51470164434615029 ) ) ;
#4485 = AXIS2_PLACEMENT_3D ( 'NONE', #2732, #6436, #2876 ) ;
#4486 = VECTOR ( 'NONE', #2729, 1000.000000000000000 ) ;
#4487 = EDGE_CURVE ( 'NONE', #5005, #3643, #4257, .T. ) ;
#4488 = AXIS2_PLACEMENT_3D ( 'NONE', #8371, #4717, #5985 ) ;
#4489 = AXIS2_PLACEMENT_3D ( 'NONE', #2697, #5267, #6735 ) ;
#4490 = CARTESIAN_POINT ( 'NONE',  ( 31.00000000000000711, 27.42469319230600533, -6.000000000000006217 ) ) ;
#4491 = CARTESIAN_POINT ( 'NONE',  ( -15.25056439471426195, 60.99999999999999289, 27.56211685706803038 ) ) ;
#4492 = EDGE_CURVE ( 'NONE', #9092, #3225, #5578, .T. ) ;
#4493 = ORIENTED_EDGE ( 'NONE', *, *, #6050, .F. ) ;
#4494 = DIRECTION ( 'NONE',  ( 0.000000000000000000, 0.000000000000000000, -1.000000000000000000 ) ) ;
#4495 = CARTESIAN_POINT ( 'NONE',  ( 8.237197373723113003, -15.00000000000000000, 27.80554943579302929 ) ) ;
#4496 = EDGE_CURVE ( 'NONE', #1980, #9059, #6759, .T. ) ;
#4497 = ORIENTED_EDGE ( 'NONE', *, *, #8395, .T. ) ;
#4498 = CIRCLE ( 'NONE', #4028, 37.00000000000000711 ) ;
#4499 = CARTESIAN_POINT ( 'NONE',  ( -0.1666666666666679342, 60.00000000000029843, -25.98601329718323782 ) ) ;
#4500 = CARTESIAN_POINT ( 'NONE',  ( -29.82695610816121956, 54.99999999999999289, 23.54469556655648432 ) ) ;
#4501 = VERTEX_POINT ( 'NONE', #7047 ) ;
#4502 = CARTESIAN_POINT ( 'NONE',  ( 9.461646124974400607, 0.04132284101285077504, 41.64849753988102066 ) ) ;
#4503 = AXIS2_PLACEMENT_3D ( 'NONE', #2316, #6713, #947 ) ;
#4504 = PRODUCT_CONTEXT ( 'NONE', #8652, 'mechanical' ) ;
#4505 = AXIS2_PLACEMENT_3D ( 'NONE', #4467, #8166, #1397 ) ;
#4506 = ORIENTED_EDGE ( 'NONE', *, *, #4513, .T. ) ;
#4507 = CARTESIAN_POINT ( 'NONE',  ( 4.000000000000001776, 0.000000000000000000, -29.00000000000000355 ) ) ;
#4508 = EDGE_CURVE ( 'NONE', #3264, #9481, #2460, .T. ) ;
#4509 = CARTESIAN_POINT ( 'NONE',  ( -5.999999999999998224, -10.00000000000000533, 31.00000000000000711 ) ) ;
#4510 = EDGE_CURVE ( 'NONE', #8890, #4111, #4114, .T. ) ;
#4511 = VERTEX_POINT ( 'NONE', #7751 ) ;
#4512 = DIRECTION ( 'NONE',  ( 0.000000000000000000, 0.000000000000000000, 1.000000000000000000 ) ) ;
#4513 = EDGE_CURVE ( 'NONE', #8621, #5790, #263, .T. ) ;
#4514 = VERTEX_POINT ( 'NONE', #3301 ) ;
#4515 = AXIS2_PLACEMENT_3D ( 'NONE', #7057, #7961, #1976 ) ;
#4516 = CARTESIAN_POINT ( 'NONE',  ( -0.3130905416343935377, 13.29544676968441053, 44.00030389938851272 ) ) ;
#4517 = AXIS2_PLACEMENT_3D ( 'NONE', #6178, #1697, #7625 ) ;
#4518 = DIRECTION ( 'NONE',  ( -0.000000000000000000, 0.000000000000000000, 1.000000000000000000 ) ) ;
#4519 = AXIS2_PLACEMENT_3D ( 'NONE', #9021, #1563, #3633 ) ;
#4520 = PRESENTATION_LAYER_ASSIGNMENT (  '', '', ( #6071 ) ) ;
#4521 = LINE ( 'NONE', #616, #6972 ) ;
#4522 = AXIS2_PLACEMENT_3D ( 'NONE', #1566, #1754, #3131 ) ;
#4523 = ORIENTED_EDGE ( 'NONE', *, *, #8261, .F. ) ;
#4524 = FACE_OUTER_BOUND ( 'NONE', #1983, .T. ) ;
#4525 = EDGE_LOOP ( 'NONE', ( #2247, #9388, #7251, #314 ) ) ;
#4526 = EDGE_LOOP ( 'NONE', ( #1247, #8736 ) ) ;
#4527 = CARTESIAN_POINT ( 'NONE',  ( -5.562309845534584518, 60.99999999999999289, 30.56426808735054124 ) ) ;
#4528 =( LENGTH_UNIT ( ) NAMED_UNIT ( * ) SI_UNIT ( .MILLI., .METRE. ) );
#4529 = DIRECTION ( 'NONE',  ( -1.820952055660014662E-28, -1.000000000000000000, -7.038118388768679669E-30 ) ) ;
#4530 = CARTESIAN_POINT ( 'NONE',  ( 0.000000000000000000, 61.99999999999999289, 0.000000000000000000 ) ) ;
#4531 = CIRCLE ( 'NONE', #8626, 1.610000000000000098 ) ;
#4532 = PLANE ( 'NONE',  #9196 ) ;
#4533 = ADVANCED_FACE ( 'NONE', ( #6310 ), #6924, .F. ) ;
#4534 = CARTESIAN_POINT ( 'NONE',  ( 9.082100980773736509, 61.99999999999999289, -35.86802812777734317 ) ) ;
#4535 = ORIENTED_EDGE ( 'NONE', *, *, #5013, .T. ) ;
#4536 = DIRECTION ( 'NONE',  ( 0.000000000000000000, 1.000000000000000000, 0.000000000000000000 ) ) ;
#4537 = CARTESIAN_POINT ( 'NONE',  ( -2.094888803305880518E-13, 59.99999999999999289, 30.00000000000000711 ) ) ;
#4538 = DIRECTION ( 'NONE',  ( -0.000000000000000000, -1.000000000000000000, -0.000000000000000000 ) ) ;
#4539 = FACE_OUTER_BOUND ( 'NONE', #607, .T. ) ;
#4540 = LINE ( 'NONE', #6787, #5161 ) ;
#4541 = DIRECTION ( 'NONE',  ( -0.000000000000000000, -1.000000000000000000, -0.000000000000000000 ) ) ;
#4542 = VERTEX_POINT ( 'NONE', #2883 ) ;
#4543 = DIRECTION ( 'NONE',  ( -1.000000000000000000, 0.000000000000000000, -0.000000000000000000 ) ) ;
#4544 = DIRECTION ( 'NONE',  ( -0.000000000000000000, -1.000000000000000000, -0.000000000000000000 ) ) ;
#4545 = ORIENTED_EDGE ( 'NONE', *, *, #1305, .T. ) ;
#4546 = CARTESIAN_POINT ( 'NONE',  ( 1.300000000000000044, 0.7216878364870328300, -1.250000000000000000 ) ) ;
#4547 = CARTESIAN_POINT ( 'NONE',  ( 2.800868546665862269, -15.00000000000000000, 29.90216386052837549 ) ) ;
#4548 = ORIENTED_EDGE ( 'NONE', *, *, #6420, .F. ) ;
#4549 = DIRECTION ( 'NONE',  ( -0.000000000000000000, 1.000000000000000000, -0.000000000000000000 ) ) ;
#4550 = FACE_OUTER_BOUND ( 'NONE', #6700, .T. ) ;
#4551 = VERTEX_POINT ( 'NONE', #8970 ) ;
#4552 = CARTESIAN_POINT ( 'NONE',  ( 9.839714455520448766, 5.126572604364064034, 37.89933748290150817 ) ) ;
#4553 = APPLICATION_PROTOCOL_DEFINITION ( 'draft international standard', 'automotive_design', 1998, #709 ) ;
#4554 = ORIENTED_EDGE ( 'NONE', *, *, #4797, .T. ) ;
#4555 = CARTESIAN_POINT ( 'NONE',  ( -28.34870838944214455, 59.99999999999999289, -9.815840903884556212 ) ) ;
#4556 = DIRECTION ( 'NONE',  ( -1.000000000000000000, -0.000000000000000000, -0.000000000000000000 ) ) ;
#4557 = VERTEX_POINT ( 'NONE', #8176 ) ;
#4558 = CARTESIAN_POINT ( 'NONE',  ( 9.860132971832495485, 39.99999999999999289, 28.33333333333341031 ) ) ;
#4559 = ORIENTED_EDGE ( 'NONE', *, *, #4393, .T. ) ;
#4560 = CARTESIAN_POINT ( 'NONE',  ( -0.9994180975881532536, 27.99999999999992895, -31.00000000000001066 ) ) ;
#4561 = CARTESIAN_POINT ( 'NONE',  ( -8.216777476527294510, 57.50000000000029843, -23.61111111111111427 ) ) ;
#4562 = DIRECTION ( 'NONE',  ( 0.000000000000000000, -1.000000000000000000, 0.000000000000000000 ) ) ;
#4563 = EDGE_CURVE ( 'NONE', #3415, #7610, #1455, .T. ) ;
#4564 = EDGE_CURVE ( 'NONE', #9118, #4597, #5854, .T. ) ;
#4565 = EDGE_CURVE ( 'NONE', #341, #7014, #4156, .T. ) ;
#4566 = VECTOR ( 'NONE', #580, 1000.000000000000000 ) ;
#4567 = ORIENTED_EDGE ( 'NONE', *, *, #8185, .T. ) ;
#4568 = CARTESIAN_POINT ( 'NONE',  ( -0.02206928620401079830, -9.470079073673241865, 39.52734620791224529 ) ) ;
#4569 = VERTEX_POINT ( 'NONE', #4133 ) ;
#4570 = UNCERTAINTY_MEASURE_WITH_UNIT (LENGTH_MEASURE( 1.000000000000000082E-05 ), #2176, 'distance_accuracy_value', 'NONE');
#4571 = ORIENTED_EDGE ( 'NONE', *, *, #6237, .T. ) ;
#4572 = FACE_OUTER_BOUND ( 'NONE', #6301, .T. ) ;
#4573 = CARTESIAN_POINT ( 'NONE',  ( -1.936180212574767801, -6.526933022534523232, 38.96892306166470377 ) ) ;
#4574 = CARTESIAN_POINT ( 'NONE',  ( 0.000000000000000000, -10.00000000000000533, 0.000000000000000000 ) ) ;
#4575 = DIRECTION ( 'NONE',  ( 0.000000000000000000, 0.000000000000000000, 1.000000000000000000 ) ) ;
#4576 = EDGE_CURVE ( 'NONE', #9368, #2152, #2689, .T. ) ;
#4577 = AXIS2_PLACEMENT_3D ( 'NONE', #5752, #7186, #7933 ) ;
#4578 = PRODUCT_DEFINITION_SHAPE ( 'NONE', 'NONE',  #8871 ) ;
#4579 = EDGE_CURVE ( 'NONE', #6748, #5855, #1166, .T. ) ;
#4580 = ORIENTED_EDGE ( 'NONE', *, *, #74, .T. ) ;
#4581 = DIRECTION ( 'NONE',  ( 0.000000000000000000, 0.000000000000000000, 1.000000000000000000 ) ) ;
#4582 = DIRECTION ( 'NONE',  ( 0.000000000000000000, 1.000000000000000000, 0.000000000000000000 ) ) ;
#4583 = ORIENTED_EDGE ( 'NONE', *, *, #1951, .F. ) ;
#4584 = CARTESIAN_POINT ( 'NONE',  ( -8.634329568050702619, 61.97962948615073486, 36.36986309197412481 ) ) ;
#4585 = DIRECTION ( 'NONE',  ( 0.000000000000000000, 0.000000000000000000, -1.000000000000000000 ) ) ;
#4586 = DIRECTION ( 'NONE',  ( -1.820952055660014662E-28, -1.000000000000000000, -7.038118388768679669E-30 ) ) ;
#4587 = CARTESIAN_POINT ( 'NONE',  ( 6.397328100368729231, 58.99819947112212759, -35.43017184758411986 ) ) ;
#4588 = CARTESIAN_POINT ( 'NONE',  ( -3.482141448764432212, -15.00000000000000000, 29.62376806748125446 ) ) ;
#4589 = DIRECTION ( 'NONE',  ( 1.735493991486225972E-29, -6.508102468073347395E-30, -1.000000000000000000 ) ) ;
#4590 = CARTESIAN_POINT ( 'NONE',  ( -5.999999999999998224, 30.00000000000000000, 28.37252191822216218 ) ) ;
#4591 = EDGE_LOOP ( 'NONE', ( #3897, #7179 ) ) ;
#4592 = VECTOR ( 'NONE', #5897, 1000.000000000000000 ) ;
#4593 = CIRCLE ( 'NONE', #415, 27.00000000000000355 ) ;
#4594 = CARTESIAN_POINT ( 'NONE',  ( 10.84614626901677248, 54.99999999999999289, 31.16666666666639784 ) ) ;
#4595 = AXIS2_PLACEMENT_3D ( 'NONE', #6727, #8031, #1267 ) ;
#4596 = CARTESIAN_POINT ( 'NONE',  ( 20.44670930779908247, 54.99999999999999289, 25.90235662024525709 ) ) ;
#4597 = VERTEX_POINT ( 'NONE', #2788 ) ;
#4598 = CARTESIAN_POINT ( 'NONE',  ( -5.137569555611031014, 60.99999999999999289, -32.59762842694632212 ) ) ;
#4599 = CARTESIAN_POINT ( 'NONE',  ( 1.425420758115970354, -14.99999999999999822, 30.37403179307458601 ) ) ;
#4600 = ADVANCED_FACE ( 'NONE', ( #5949 ), #7486, .T. ) ;
#4601 = ORIENTED_EDGE ( 'NONE', *, *, #6768, .T. ) ;
#4602 = AXIS2_PLACEMENT_3D ( 'NONE', #8142, #9079, #680 ) ;
#4603 = CARTESIAN_POINT ( 'NONE',  ( 1.300000000000000044, 0.7216878364870328300, -1.250000000000000000 ) ) ;
#4604 = EDGE_CURVE ( 'NONE', #8554, #3204, #1416, .T. ) ;
#4605 = CARTESIAN_POINT ( 'NONE',  ( 3.903202352150908272, 61.96703986863185776, -37.25258870257768251 ) ) ;
#4606 = ORIENTED_EDGE ( 'NONE', *, *, #5776, .F. ) ;
#4607 = CARTESIAN_POINT ( 'NONE',  ( 13.20615709665468529, 1.297055670843870301, 36.69647536524409048 ) ) ;
#4608 = AXIS2_PLACEMENT_3D ( 'NONE', #8056, #3608, #7310 ) ;
#4609 = VERTEX_POINT ( 'NONE', #2091 ) ;
#4610 = LINE ( 'NONE', #2260, #6554 ) ;
#4611 = DIRECTION ( 'NONE',  ( 0.000000000000000000, 0.000000000000000000, -1.000000000000000000 ) ) ;
#4612 = CARTESIAN_POINT ( 'NONE',  ( 0.000000000000000000, 58.99999999999999289, 0.000000000000000000 ) ) ;
#4613 = ORIENTED_EDGE ( 'NONE', *, *, #7886, .T. ) ;
#4614 = CARTESIAN_POINT ( 'NONE',  ( -12.16083066526041989, 40.00000000000014921, -34.94444444444444287 ) ) ;
#4615 = ORIENTED_EDGE ( 'NONE', *, *, #7286, .T. ) ;
#4616 = CARTESIAN_POINT ( 'NONE',  ( -7.921576059427342997, 9.406609150246151074, 42.36640274441228371 ) ) ;
#4617 = PLANE ( 'NONE',  #8715 ) ;
#4618 = DIRECTION ( 'NONE',  ( -0.000000000000000000, 1.000000000000000000, -0.000000000000000000 ) ) ;
#4619 = EDGE_CURVE ( 'NONE', #1358, #6132, #2989, .T. ) ;
#4620 = CIRCLE ( 'NONE', #976, 1.500000000000001332 ) ;
#4621 = VERTEX_POINT ( 'NONE', #8821 ) ;
#4622 = CARTESIAN_POINT ( 'NONE',  ( 4.776122516674679455E-15, 19.99999999999982236, -39.00000000000002132 ) ) ;
#4623 = DIRECTION ( 'NONE',  ( -1.000000000000000000, 0.000000000000000000, 1.084202172485503448E-16 ) ) ;
#4624 = ORIENTED_EDGE ( 'NONE', *, *, #6232, .T. ) ;
#4625 = ORIENTED_EDGE ( 'NONE', *, *, #2723, .F. ) ;
#4626 = CARTESIAN_POINT ( 'NONE',  ( 5.562309845534932684, 60.99999999999999289, -33.06426808735049150 ) ) ;
#4627 = CIRCLE ( 'NONE', #1149, 19.00000000000005684 ) ;
#4628 = ADVANCED_FACE ( 'NONE', ( #7152 ), #8082, .T. ) ;
#4629 = FACE_OUTER_BOUND ( 'NONE', #2742, .T. ) ;
#4630 = DIRECTION ( 'NONE',  ( -0.000000000000000000, -1.000000000000000000, -0.000000000000000000 ) ) ;
#4631 = VECTOR ( 'NONE', #7026, 1000.000000000000000 ) ;
#4632 = VERTEX_POINT ( 'NONE', #1138 ) ;
#4633 = CARTESIAN_POINT ( 'NONE',  ( -32.92587516511807166, 59.99999999999999289, -3.065181147996824507 ) ) ;
#4634 = DIRECTION ( 'NONE',  ( -0.000000000000000000, -1.000000000000000000, -0.000000000000000000 ) ) ;
#4635 = AXIS2_PLACEMENT_3D ( 'NONE', #3696, #7504, #1625 ) ;
#4636 = ORIENTED_EDGE ( 'NONE', *, *, #1676, .F. ) ;
#4637 = CARTESIAN_POINT ( 'NONE',  ( 4.460510837761463065, -5.679267476043179386, 43.49797445894572689 ) ) ;
#4638 = LINE ( 'NONE', #1616, #4990 ) ;
#4639 = EDGE_CURVE ( 'NONE', #5003, #4849, #1319, .T. ) ;
#4640 = CARTESIAN_POINT ( 'NONE',  ( 2.805732460449232857, -15.00000000000000000, 29.91534241968305352 ) ) ;
#4641 = FACE_OUTER_BOUND ( 'NONE', #4180, .T. ) ;
#4642 = EDGE_CURVE ( 'NONE', #5205, #6457, #6331, .T. ) ;
#4643 = FACE_OUTER_BOUND ( 'NONE', #5834, .T. ) ;
#4644 = EDGE_LOOP ( 'NONE', ( #1629, #8480, #2506, #7156 ) ) ;
#4645 = CARTESIAN_POINT ( 'NONE',  ( -31.00000000000001066, 27.75862132583096553, 4.003261267919811850 ) ) ;
#4646 = DIRECTION ( 'NONE',  ( -0.000000000000000000, -1.000000000000000000, -0.000000000000000000 ) ) ;
#4647 = ORIENTED_EDGE ( 'NONE', *, *, #1288, .T. ) ;
#4648 = CARTESIAN_POINT ( 'NONE',  ( 20.99999999999999645, 0.000000000000000000, 4.000000000000000888 ) ) ;
#4649 = CARTESIAN_POINT ( 'NONE',  ( 4.904043666719842598, 60.99999999999999289, 31.11591804390326743 ) ) ;
#4650 = ORIENTED_EDGE ( 'NONE', *, *, #1775, .F. ) ;
#4651 = CARTESIAN_POINT ( 'NONE',  ( 0.000000000000000000, 61.99999999999999289, -37.00000000000001421 ) ) ;
#4652 = CIRCLE ( 'NONE', #2266, 26.00000000000004974 ) ;
#4653 = DIRECTION ( 'NONE',  ( 0.000000000000000000, 0.000000000000000000, 1.000000000000000000 ) ) ;
#4654 = ORIENTED_EDGE ( 'NONE', *, *, #3911, .T. ) ;
#4655 = CARTESIAN_POINT ( 'NONE',  ( 6.080049472934138777, -4.651243486359556201, 43.04620881594706105 ) ) ;
#4656 = EDGE_LOOP ( 'NONE', ( #4165, #1778, #4767, #3391 ) ) ;
#4657 = CARTESIAN_POINT ( 'NONE',  ( 5.000000000000002665, 30.00000000000000000, -30.00000000000000711 ) ) ;
#4658 = VECTOR ( 'NONE', #2237, 1000.000000000000000 ) ;
#4659 = DIRECTION ( 'NONE',  ( 0.000000000000000000, 0.000000000000000000, -1.000000000000000000 ) ) ;
#4660 = ORIENTED_EDGE ( 'NONE', *, *, #5889, .T. ) ;
#4661 = CARTESIAN_POINT ( 'NONE',  ( 0.000000000000000000, 0.000000000000000000, 0.000000000000000000 ) ) ;
#4662 = ORIENTED_EDGE ( 'NONE', *, *, #5037, .F. ) ;
#4663 = DIRECTION ( 'NONE',  ( 1.000000000000000000, 0.000000000000000000, -2.168404344971006649E-16 ) ) ;
#4664 = CARTESIAN_POINT ( 'NONE',  ( -3.903202352150655585, 61.96703986863184355, 37.25258870257768962 ) ) ;
#4665 = CIRCLE ( 'NONE', #7009, 37.99999999999999289 ) ;
#4666 = VECTOR ( 'NONE', #1317, 1000.000000000000000 ) ;
#4667 = ORIENTED_EDGE ( 'NONE', *, *, #2239, .F. ) ;
#4668 = LINE ( 'NONE', #4020, #7978 ) ;
#4669 = CIRCLE ( 'NONE', #3238, 4.500000000000004441 ) ;
#4670 = ORIENTED_EDGE ( 'NONE', *, *, #8544, .F. ) ;
#4671 = CONICAL_SURFACE ( 'NONE', #1196, 17.99999999999999645, 0.7853981633974517207 ) ;
#4672 = AXIS2_PLACEMENT_3D ( 'NONE', #40, #6040, #3837 ) ;
#4673 = ORIENTED_EDGE ( 'NONE', *, *, #7943, .T. ) ;
#4674 = AXIS2_PLACEMENT_3D ( 'NONE', #1564, #8332, #4585 ) ;
#4675 = AXIS2_PLACEMENT_3D ( 'NONE', #1846, #4863, #2629 ) ;
#4676 = CARTESIAN_POINT ( 'NONE',  ( -3.485699947575983781, -11.18892459271980577, 38.84620403412360190 ) ) ;
#4677 =( NAMED_UNIT ( * ) SI_UNIT ( $, .STERADIAN. ) SOLID_ANGLE_UNIT ( ) );
#4678 = FACE_OUTER_BOUND ( 'NONE', #7061, .T. ) ;
#4679 = VECTOR ( 'NONE', #5053, 1000.000000000000000 ) ;
#4680 = AXIS2_PLACEMENT_3D ( 'NONE', #8458, #7753, #9382 ) ;
#4681 = ORIENTED_EDGE ( 'NONE', *, *, #3349, .F. ) ;
#4682 = DIRECTION ( 'NONE',  ( -0.000000000000000000, -1.000000000000000000, -0.000000000000000000 ) ) ;
#4683 = ORIENTED_EDGE ( 'NONE', *, *, #1832, .T. ) ;
#4684 = DIRECTION ( 'NONE',  ( 0.000000000000000000, 0.000000000000000000, -1.000000000000000000 ) ) ;
#4685 = CARTESIAN_POINT ( 'NONE',  ( 7.420105108763668689, 59.31303094616893645, -34.74949143486232828 ) ) ;
#4686 = CIRCLE ( 'NONE', #1838, 3.799999999999999378 ) ;
#4687 = CARTESIAN_POINT ( 'NONE',  ( -8.216777476527294510, 56.00000000000030553, -23.61111111111111427 ) ) ;
#4688 = CARTESIAN_POINT ( 'NONE',  ( 1.313076780747179484, 18.23965141680392321, 38.98324215956266414 ) ) ;
#4689 = CARTESIAN_POINT ( 'NONE',  ( 29.82695610816121956, 39.99999999999999289, -23.54469556655648077 ) ) ;
#4690 = ORIENTED_EDGE ( 'NONE', *, *, #4328, .F. ) ;
#4691 = LINE ( 'NONE', #974, #1968 ) ;
#4692 = EDGE_CURVE ( 'NONE', #64, #7439, #172, .T. ) ;
#4693 = EDGE_CURVE ( 'NONE', #2443, #5928, #8925, .T. ) ;
#4694 = EDGE_CURVE ( 'NONE', #9299, #4234, #8521, .T. ) ;
#4695 = EDGE_CURVE ( 'NONE', #8444, #4597, #2937, .T. ) ;
#4696 = ORIENTED_EDGE ( 'NONE', *, *, #5051, .T. ) ;
#4697 = DIRECTION ( 'NONE',  ( 1.735493991486227373E-29, 0.000000000000000000, -1.000000000000000000 ) ) ;
#4698 = ORIENTED_EDGE ( 'NONE', *, *, #2373, .T. ) ;
#4699 = FACE_BOUND ( 'NONE', #543, .T. ) ;
#4700 = CARTESIAN_POINT ( 'NONE',  ( 1.040310318760209318E-26, 47.50000000000033396, -25.00000000000000000 ) ) ;
#4701 = ORIENTED_EDGE ( 'NONE', *, *, #7565, .T. ) ;
#4702 = DIRECTION ( 'NONE',  ( 0.000000000000000000, 0.000000000000000000, 1.000000000000000000 ) ) ;
#4703 = CARTESIAN_POINT ( 'NONE',  ( -27.56211685706797709, 61.99999999999999289, -15.25056439471436676 ) ) ;
#4704 = CARTESIAN_POINT ( 'NONE',  ( 1.300547793265065533, -6.641803996390986953, 43.96733177750241595 ) ) ;
#4705 = DIRECTION ( 'NONE',  ( -1.000000000000000000, -0.000000000000000000, -0.000000000000000000 ) ) ;
#4706 = DIRECTION ( 'NONE',  ( 0.000000000000000000, 0.000000000000000000, 1.000000000000000000 ) ) ;
#4707 = CARTESIAN_POINT ( 'NONE',  ( -15.97678174684350871, 60.99999999999999289, 28.87459861216650836 ) ) ;
#4708 = DIRECTION ( 'NONE',  ( -1.000000000000000000, 0.000000000000000000, 0.000000000000000000 ) ) ;
#4709 = ORIENTED_EDGE ( 'NONE', *, *, #5282, .T. ) ;
#4710 = FACE_OUTER_BOUND ( 'NONE', #6962, .T. ) ;
#4711 = CARTESIAN_POINT ( 'NONE',  ( -3.332326962091669120, 61.99999999999999289, 36.97859170863238631 ) ) ;
#4712 = ORIENTED_EDGE ( 'NONE', *, *, #6721, .F. ) ;
#4713 = CARTESIAN_POINT ( 'NONE',  ( -2.083000153361134643, -9.308704936926149642, 39.45524585924379579 ) ) ;
#4714 = ORIENTED_EDGE ( 'NONE', *, *, #4249, .T. ) ;
#4715 = ORIENTED_EDGE ( 'NONE', *, *, #3189, .T. ) ;
#4716 = EDGE_CURVE ( 'NONE', #137, #6352, #325, .T. ) ;
#4717 = DIRECTION ( 'NONE',  ( -1.000000000000000000, 0.000000000000000000, 0.000000000000000000 ) ) ;
#4718 = FACE_OUTER_BOUND ( 'NONE', #6328, .T. ) ;
#4719 = DIRECTION ( 'NONE',  ( -0.000000000000000000, -1.000000000000000000, -0.000000000000000000 ) ) ;
#4720 = EDGE_CURVE ( 'NONE', #7878, #4449, #7543, .T. ) ;
#4721 = ORIENTED_EDGE ( 'NONE', *, *, #983, .F. ) ;
#4722 = CYLINDRICAL_SURFACE ( 'NONE', #637, 1.500000000000001332 ) ;
#4723 = DIRECTION ( 'NONE',  ( -0.000000000000000000, 1.000000000000000000, 0.000000000000000000 ) ) ;
#4724 = ORIENTED_EDGE ( 'NONE', *, *, #8103, .F. ) ;
#4725 = LINE ( 'NONE', #7733, #6322 ) ;
#4726 = CARTESIAN_POINT ( 'NONE',  ( 3.265277612493203918, 59.85134567364465141, -34.06652594440189574 ) ) ;
#4727 = DIRECTION ( 'NONE',  ( 0.000000000000000000, 0.000000000000000000, 1.000000000000000000 ) ) ;
#4728 =( NAMED_UNIT ( * ) PLANE_ANGLE_UNIT ( ) SI_UNIT ( $, .RADIAN. ) );
#4729 = DIRECTION ( 'NONE',  ( -0.000000000000000000, -1.000000000000000000, -0.000000000000000000 ) ) ;
#4730 = ORIENTED_EDGE ( 'NONE', *, *, #3124, .F. ) ;
#4731 = DIRECTION ( 'NONE',  ( 0.000000000000000000, 0.000000000000000000, 1.000000000000000000 ) ) ;
#4732 = CIRCLE ( 'NONE', #9618, 1.500000000000001332 ) ;
#4733 = EDGE_CURVE ( 'NONE', #2965, #2351, #6881, .T. ) ;
#4734 = CARTESIAN_POINT ( 'NONE',  ( 24.67792535850613334, 28.99999999999997158, 4.000000000000000888 ) ) ;
#4735 = VECTOR ( 'NONE', #8629, 1000.000000000000341 ) ;
#4736 = ORIENTED_EDGE ( 'NONE', *, *, #5087, .T. ) ;
#4737 = DIRECTION ( 'NONE',  ( 2.168404344971006649E-16, 0.000000000000000000, 1.000000000000000000 ) ) ;
#4738 = PRODUCT_DEFINITION_SHAPE ( 'NONE', 'NONE',  #8147 ) ;
#4739 = ORIENTED_EDGE ( 'NONE', *, *, #4733, .T. ) ;
#4740 = LINE ( 'NONE', #4098, #3029 ) ;
#4741 = CARTESIAN_POINT ( 'NONE',  ( 37.54740336257584232, 61.81808349686849624, 6.037872445562960877 ) ) ;
#4742 = ORIENTED_EDGE ( 'NONE', *, *, #5995, .T. ) ;
#4743 = EDGE_CURVE ( 'NONE', #185, #2421, #3126, .T. ) ;
#4744 = EDGE_CURVE ( 'NONE', #7534, #880, #1385, .T. ) ;
#4745 = CARTESIAN_POINT ( 'NONE',  ( 0.000000000000000000, 60.99999999999999289, 0.000000000000000000 ) ) ;
#4746 = AXIS2_PLACEMENT_3D ( 'NONE', #7986, #4238, #8726 ) ;
#4747 = CARTESIAN_POINT ( 'NONE',  ( -37.55900191124520404, 61.85658167520826822, -5.210294541070858543 ) ) ;
#4748 = VERTEX_POINT ( 'NONE', #89 ) ;
#4749 = DIRECTION ( 'NONE',  ( 0.000000000000000000, 0.000000000000000000, 1.000000000000000000 ) ) ;
#4750 = DIRECTION ( 'NONE',  ( -0.000000000000000000, -1.000000000000000000, -0.000000000000000000 ) ) ;
#4751 = ADVANCED_FACE ( 'NONE', ( #6778 ), #967, .F. ) ;
#4752 = AXIS2_PLACEMENT_3D ( 'NONE', #7262, #4902, #8844 ) ;
#4753 = VERTEX_POINT ( 'NONE', #3932 ) ;
#4754 = CARTESIAN_POINT ( 'NONE',  ( 1.300000000000000044, -0.7216878364870317197, -1.250000000000000000 ) ) ;
#4755 = EDGE_LOOP ( 'NONE', ( #1153, #5150, #2065, #2776 ) ) ;
#4756 = DIRECTION ( 'NONE',  ( 0.000000000000000000, 0.000000000000000000, 1.000000000000000000 ) ) ;
#4757 = EDGE_LOOP ( 'NONE', ( #3343, #3479, #5349, #4667 ) ) ;
#4758 = ADVANCED_FACE ( 'NONE', ( #5368 ), #6140, .F. ) ;
#4759 = EDGE_CURVE ( 'NONE', #252, #2338, #4269, .T. ) ;
#4760 = CARTESIAN_POINT ( 'NONE',  ( 5.423418723394456162E-28, -2.066522830327504070E-28, -26.00000000000003197 ) ) ;
#4761 = CARTESIAN_POINT ( 'NONE',  ( -9.463197482281705319, 0.04576215439031022097, 41.64770477980678010 ) ) ;
#4762 = ADVANCED_FACE ( 'NONE', ( #4283 ), #7281, .T. ) ;
#4763 = ORIENTED_EDGE ( 'NONE', *, *, #8070, .T. ) ;
#4764 = CARTESIAN_POINT ( 'NONE',  ( -34.92646553026882117, 59.22976218012610161, -7.237999934912877187 ) ) ;
#4765 = VERTEX_POINT ( 'NONE', #4534 ) ;
#4766 = DIRECTION ( 'NONE',  ( -1.000000000000000000, 0.000000000000000000, 0.000000000000000000 ) ) ;
#4767 = ORIENTED_EDGE ( 'NONE', *, *, #8796, .F. ) ;
#4768 = ORIENTED_EDGE ( 'NONE', *, *, #5585, .F. ) ;
#4769 = CARTESIAN_POINT ( 'NONE',  ( -9.999521393725496310, 3.638235021868027719, 41.36449609663748106 ) ) ;
#4770 = EDGE_CURVE ( 'NONE', #1752, #2376, #7588, .T. ) ;
#4771 = DIRECTION ( 'NONE',  ( 0.000000000000000000, 0.000000000000000000, 1.000000000000000000 ) ) ;
#4772 = AXIS2_PLACEMENT_3D ( 'NONE', #7595, #8384, #8334 ) ;
#4773 = CARTESIAN_POINT ( 'NONE',  ( -28.33333333333344939, 59.99999999999999289, 9.860132971832396009 ) ) ;
#4774 = ADVANCED_FACE ( 'NONE', ( #9171 ), #3028, .F. ) ;
#4775 = ORIENTED_EDGE ( 'NONE', *, *, #7943, .F. ) ;
#4776 = LINE ( 'NONE', #7782, #4735 ) ;
#4777 = ORIENTED_EDGE ( 'NONE', *, *, #8008, .T. ) ;
#4778 = FACE_OUTER_BOUND ( 'NONE', #4860, .T. ) ;
#4779 = AXIS2_PLACEMENT_3D ( 'NONE', #7903, #4001, #2648 ) ;
#4780 = CARTESIAN_POINT ( 'NONE',  ( 8.070750150710592763, 59.89221580632705155, -33.08193339022353996 ) ) ;
#4781 = DIRECTION ( 'NONE',  ( 0.000000000000000000, 1.000000000000000000, 0.000000000000000000 ) ) ;
#4782 = FILL_AREA_STYLE ('',( #3280 ) ) ;
#4783 = DIRECTION ( 'NONE',  ( -1.000000000000000000, -0.000000000000000000, -0.000000000000000000 ) ) ;
#4784 = CARTESIAN_POINT ( 'NONE',  ( -31.00000000000000711, 27.42469319230600533, 6.000000000000009770 ) ) ;
#4785 = VECTOR ( 'NONE', #1212, 1000.000000000000000 ) ;
#4786 = CIRCLE ( 'NONE', #2853, 2.500000000000002220 ) ;
#4787 = FACE_OUTER_BOUND ( 'NONE', #7466, .T. ) ;
#4788 = VERTEX_POINT ( 'NONE', #2288 ) ;
#4789 = DIRECTION ( 'NONE',  ( 0.000000000000000000, 0.000000000000000000, -1.000000000000000000 ) ) ;
#4790 = LINE ( 'NONE', #4099, #587 ) ;
#4791 = CIRCLE ( 'NONE', #542, 5.000000000000001776 ) ;
#4792 = VERTEX_POINT ( 'NONE', #9072 ) ;
#4793 = CYLINDRICAL_SURFACE ( 'NONE', #3699, 1.500000000000001332 ) ;
#4794 = EDGE_CURVE ( 'NONE', #9521, #7758, #5975, .T. ) ;
#4795 = CARTESIAN_POINT ( 'NONE',  ( -5.562309845534700870, 60.99999999999999289, 28.56426808735051992 ) ) ;
#4796 = DIRECTION ( 'NONE',  ( 1.000000000000000000, -0.000000000000000000, 0.000000000000000000 ) ) ;
#4797 = EDGE_CURVE ( 'NONE', #6432, #3019, #5523, .T. ) ;
#4798 = CARTESIAN_POINT ( 'NONE',  ( -0.02610464500743471528, -11.70511861050984947, 38.99999126342864741 ) ) ;
#4799 = VERTEX_POINT ( 'NONE', #2386 ) ;
#4800 = DIRECTION ( 'NONE',  ( 0.000000000000000000, 1.000000000000000000, 0.000000000000000000 ) ) ;
#4801 = ORIENTED_EDGE ( 'NONE', *, *, #1707, .T. ) ;
#4802 = CARTESIAN_POINT ( 'NONE',  ( -5.562309845534700870, 61.99999999999999289, 28.56426808735051992 ) ) ;
#4803 = CARTESIAN_POINT ( 'NONE',  ( 0.000000000000000000, 59.99999999999999289, 0.000000000000000000 ) ) ;
#4804 = ORIENTED_EDGE ( 'NONE', *, *, #5225, .F. ) ;
#4805 = VECTOR ( 'NONE', #785, 1000.000000000000000 ) ;
#4806 = LINE ( 'NONE', #4166, #8397 ) ;
#4807 = DIRECTION ( 'NONE',  ( -1.735493991486225972E-29, 6.508102468073347395E-30, 1.000000000000000000 ) ) ;
#4808 = ADVANCED_FACE ( 'NONE', ( #3888 ), #4722, .F. ) ;
#4809 = VECTOR ( 'NONE', #9111, 1000.000000000000000 ) ;
#4810 = EDGE_CURVE ( 'NONE', #1652, #4857, #3830, .T. ) ;
#4811 = VECTOR ( 'NONE', #4250, 1000.000000000000000 ) ;
#4812 = ORIENTED_EDGE ( 'NONE', *, *, #7761, .F. ) ;
#4813 = CARTESIAN_POINT ( 'NONE',  ( -35.56433427405016090, 59.02194934605864063, -5.394111410765020764 ) ) ;
#4814 = ADVANCED_FACE ( 'NONE', ( #6830 ), #5420, .T. ) ;
#4815 = ORIENTED_EDGE ( 'NONE', *, *, #3039, .F. ) ;
#4816 = CARTESIAN_POINT ( 'NONE',  ( -23.54759692749571087, 59.99999999999999289, 18.58791755254458877 ) ) ;
#4817 = ORIENTED_EDGE ( 'NONE', *, *, #5766, .F. ) ;
#4818 = CARTESIAN_POINT ( 'NONE',  ( -9.745578801763752352, 1.029427285159154160, 41.50076718676587006 ) ) ;
#4819 = VECTOR ( 'NONE', #753, 1000.000000000000000 ) ;
#4820 = DIRECTION ( 'NONE',  ( -0.000000000000000000, 1.000000000000000000, -0.000000000000000000 ) ) ;
#4821 = DIRECTION ( 'NONE',  ( -1.735493991486225972E-29, 6.508102468073347395E-30, 1.000000000000000000 ) ) ;
#4822 = EDGE_LOOP ( 'NONE', ( #2172, #266, #3229, #7371, #1484 ) ) ;
#4823 = AXIS2_PLACEMENT_3D ( 'NONE', #8059, #7217, #5047 ) ;
#4824 = ORIENTED_EDGE ( 'NONE', *, *, #6477, .T. ) ;
#4825 = DIRECTION ( 'NONE',  ( 0.000000000000000000, -1.000000000000000000, 0.000000000000000000 ) ) ;
#4826 = VECTOR ( 'NONE', #829, 1000.000000000000000 ) ;
#4827 = AXIS2_PLACEMENT_3D ( 'NONE', #9693, #5202, #8210 ) ;
#4828 = ORIENTED_EDGE ( 'NONE', *, *, #350, .T. ) ;
#4829 = DIRECTION ( 'NONE',  ( 0.5773502691896204020, -0.5773502691896366112, 0.5773502691896204020 ) ) ;
#4830 = CARTESIAN_POINT ( 'NONE',  ( -8.545448575588382667, 47.50000000000033396, -24.55555555555566372 ) ) ;
#4831 = LINE ( 'NONE', #8428, #6489 ) ;
#4832 = CARTESIAN_POINT ( 'NONE',  ( 0.000000000000000000, 59.99999999999999289, 0.000000000000000000 ) ) ;
#4833 = DIRECTION ( 'NONE',  ( -0.000000000000000000, 1.000000000000000000, -0.000000000000000000 ) ) ;
#4834 = CIRCLE ( 'NONE', #569, 10.00000000000001599 ) ;
#4835 = AXIS2_PLACEMENT_3D ( 'NONE', #8404, #5295, #2313 ) ;
#4836 = ORIENTED_EDGE ( 'NONE', *, *, #2851, .F. ) ;
#4837 = FACE_OUTER_BOUND ( 'NONE', #839, .T. ) ;
#4838 = PLANE ( 'NONE',  #708 ) ;
#4839 = EDGE_LOOP ( 'NONE', ( #8018, #9151, #3757, #945 ) ) ;
#4840 = FACE_OUTER_BOUND ( 'NONE', #9219, .T. ) ;
#4841 = DIRECTION ( 'NONE',  ( 0.000000000000000000, 1.000000000000000000, 0.000000000000000000 ) ) ;
#4842 = ORIENTED_EDGE ( 'NONE', *, *, #1181, .T. ) ;
#4843 = CARTESIAN_POINT ( 'NONE',  ( -13.30454745595961263, 3.637961880295645045, 36.66047841392798290 ) ) ;
#4844 = DIRECTION ( 'NONE',  ( -0.000000000000000000, -1.000000000000000000, -0.000000000000000000 ) ) ;
#4845 = AXIS2_PLACEMENT_3D ( 'NONE', #7911, #8506, #1691 ) ;
#4846 = DIRECTION ( 'NONE',  ( -1.000000000000000000, 0.000000000000000000, 0.000000000000000000 ) ) ;
#4847 = DIRECTION ( 'NONE',  ( 0.000000000000000000, 0.000000000000000000, 1.000000000000000000 ) ) ;
#4848 = CARTESIAN_POINT ( 'NONE',  ( 0.000000000000000000, 0.000000000000000000, 0.000000000000000000 ) ) ;
#4849 = VERTEX_POINT ( 'NONE', #5263 ) ;
#4850 = DIRECTION ( 'NONE',  ( -0.000000000000000000, -1.000000000000000000, -0.000000000000000000 ) ) ;
#4851 = LINE ( 'NONE', #3159, #3576 ) ;
#4852 = VERTEX_POINT ( 'NONE', #9124 ) ;
#4853 = CYLINDRICAL_SURFACE ( 'NONE', #6800, 10.00000000000001599 ) ;
#4854 = DIRECTION ( 'NONE',  ( -0.000000000000000000, -1.000000000000000000, -0.000000000000000000 ) ) ;
#4855 = VERTEX_POINT ( 'NONE', #8275 ) ;
#4856 = DIRECTION ( 'NONE',  ( -0.000000000000000000, -1.000000000000000000, -0.000000000000000000 ) ) ;
#4857 = VERTEX_POINT ( 'NONE', #8671 ) ;
#4858 = ORIENTED_EDGE ( 'NONE', *, *, #7049, .T. ) ;
#4859 = CYLINDRICAL_SURFACE ( 'NONE', #571, 26.00000000000006395 ) ;
#4860 = EDGE_LOOP ( 'NONE', ( #6546, #7292, #4624, #473 ) ) ;
#4861 = CARTESIAN_POINT ( 'NONE',  ( -10.00092682600661398, 2.650786234224241422, 41.36373161509812491 ) ) ;
#4862 = EDGE_CURVE ( 'NONE', #6026, #1665, #6619, .T. ) ;
#4863 = DIRECTION ( 'NONE',  ( 0.000000000000000000, 1.000000000000000000, 0.000000000000000000 ) ) ;
#4864 = ADVANCED_FACE ( 'NONE', ( #8718 ), #1014, .T. ) ;
#4865 = CARTESIAN_POINT ( 'NONE',  ( 31.00000000000000711, 30.00000000000000000, 6.000000000000000000 ) ) ;
#4866 = ORIENTED_EDGE ( 'NONE', *, *, #1461, .T. ) ;
#4867 = DIRECTION ( 'NONE',  ( 1.820952055660014662E-28, 1.000000000000000000, -6.508102468073347395E-30 ) ) ;
#4868 = ORIENTED_EDGE ( 'NONE', *, *, #4604, .T. ) ;
#4869 = DIRECTION ( 'NONE',  ( 1.735493991486225972E-29, -6.508102468073347395E-30, -1.000000000000000000 ) ) ;
#4870 = FACE_OUTER_BOUND ( 'NONE', #5779, .T. ) ;
#4871 = CARTESIAN_POINT ( 'NONE',  ( 1.300000000000000044, -0.7216878364870318308, 1.250000000000000000 ) ) ;
#4872 = CARTESIAN_POINT ( 'NONE',  ( 11.82328533550226446, -3.573622092248616600, 37.16487311033493768 ) ) ;
#4873 = CARTESIAN_POINT ( 'NONE',  ( 1.084683744678891232E-26, 48.50000000000033396, -37.00000000000000711 ) ) ;
#4874 = ADVANCED_FACE ( 'NONE', ( #7072 ), #1894, .T. ) ;
#4875 = CARTESIAN_POINT ( 'NONE',  ( 5.137569555611264605, 61.99999999999999289, 34.09762842694627949 ) ) ;
#4876 = ADVANCED_FACE ( 'NONE', ( #438 ), #4181, .F. ) ;
#4877 = ORIENTED_EDGE ( 'NONE', *, *, #5797, .F. ) ;
#4878 = CARTESIAN_POINT ( 'NONE',  ( 0.02765780018129053094, 18.29482697815594605, 43.99999130734107666 ) ) ;
#4879 = CARTESIAN_POINT ( 'NONE',  ( 28.33333333333337833, 39.99999999999999289, -9.860132971832594961 ) ) ;
#4880 = ORIENTED_EDGE ( 'NONE', *, *, #9311, .T. ) ;
#4881 = CARTESIAN_POINT ( 'NONE',  ( 5.902069945235307813, 61.82045560759793545, -37.56426808735049860 ) ) ;
#4882 = LINE ( 'NONE', #4291, #274 ) ;
#4883 = VERTEX_POINT ( 'NONE', #327 ) ;
#4884 = CARTESIAN_POINT ( 'NONE',  ( 0.000000000000000000, 54.99999999999999289, 0.000000000000000000 ) ) ;
#4885 = DIRECTION ( 'NONE',  ( -0.000000000000000000, -1.000000000000000000, -0.000000000000000000 ) ) ;
#4886 = DIRECTION ( 'NONE',  ( 1.000000000000000000, 0.000000000000000000, 0.000000000000000000 ) ) ;
#4887 = AXIS2_PLACEMENT_3D ( 'NONE', #5369, #1096, #1561 ) ;
#4888 = CIRCLE ( 'NONE', #632, 1.500000000000001332 ) ;
#4889 = CARTESIAN_POINT ( 'NONE',  ( 1.300000000000000044, -1.443375672974064328, -9.326206579303807412E-18 ) ) ;
#4890 = EDGE_LOOP ( 'NONE', ( #1228, #1176, #5405, #2824, #437, #8243, #3422, #4636, #8369, #7073, #9691, #26, #2590, #3926, #666, #7991, #2543, #8200, #3366, #7841, #4721, #367, #7721, #2195, #6756, #4113, #9326, #370, #5440, #8732, #6415, #3102 ) ) ;
#4891 = CARTESIAN_POINT ( 'NONE',  ( -23.54759692749571087, 59.99999999999999289, 18.58791755254458522 ) ) ;
#4892 = ADVANCED_FACE ( 'NONE', ( #5659 ), #5513, .T. ) ;
#4893 = ORIENTED_EDGE ( 'NONE', *, *, #7972, .T. ) ;
#4894 = DIRECTION ( 'NONE',  ( 0.000000000000000000, 0.000000000000000000, 1.000000000000000000 ) ) ;
#4895 = DIRECTION ( 'NONE',  ( 1.000000000000000000, 0.000000000000000000, 0.000000000000000000 ) ) ;
#4896 = EDGE_LOOP ( 'NONE', ( #6454, #8344, #5950 ) ) ;
#4897 = VECTOR ( 'NONE', #4337, 1000.000000000000000 ) ;
#4898 = PRODUCT_DEFINITION_SHAPE ( 'NONE', 'NONE',  #9759 ) ;
#4899 = CARTESIAN_POINT ( 'NONE',  ( 1.300000000000000044, 0.000000000000000000, 0.000000000000000000 ) ) ;
#4900 = CARTESIAN_POINT ( 'NONE',  ( -15.97678174684350871, 60.99999999999999289, 30.37459861216651191 ) ) ;
#4901 = PRODUCT_DEFINITION_CONTEXT ( 'detailed design', #9160, 'design' ) ;
#4902 = DIRECTION ( 'NONE',  ( 0.000000000000000000, 0.000000000000000000, 1.000000000000000000 ) ) ;
#4903 = DIRECTION ( 'NONE',  ( 0.000000000000000000, 1.000000000000000000, 0.000000000000000000 ) ) ;
#4904 = VECTOR ( 'NONE', #4541, 1000.000000000000000 ) ;
#4905 = ORIENTED_EDGE ( 'NONE', *, *, #5824, .T. ) ;
#4906 = DIRECTION ( 'NONE',  ( -0.000000000000000000, -1.000000000000000000, -0.000000000000000000 ) ) ;
#4907 = EDGE_LOOP ( 'NONE', ( #1696, #7040, #5496, #7781, #6108 ) ) ;
#4908 = DIRECTION ( 'NONE',  ( 0.000000000000000000, 0.000000000000000000, 1.000000000000000000 ) ) ;
#4909 = ORIENTED_EDGE ( 'NONE', *, *, #535, .F. ) ;
#4910 = VERTEX_POINT ( 'NONE', #1114 ) ;
#4911 = CARTESIAN_POINT ( 'NONE',  ( -6.620562216048003989, -4.206768621063721625, 42.86638935774112014 ) ) ;
#4912 = DIRECTION ( 'NONE',  ( -0.000000000000000000, 1.000000000000000000, -0.000000000000000000 ) ) ;
#4913 = VECTOR ( 'NONE', #9700, 1000.000000000000000 ) ;
#4914 = VECTOR ( 'NONE', #1069, 1000.000000000000000 ) ;
#4915 = ADVANCED_FACE ( 'NONE', ( #3273 ), #7929, .F. ) ;
#4916 = ORIENTED_EDGE ( 'NONE', *, *, #197, .T. ) ;
#4917 = CARTESIAN_POINT ( 'NONE',  ( -26.32489316217637665, -10.00000000000000533, -5.999999999999997335 ) ) ;
#4918 = VERTEX_POINT ( 'NONE', #4917 ) ;
#4919 = DIRECTION ( 'NONE',  ( 0.000000000000000000, 0.000000000000000000, -1.000000000000000000 ) ) ;
#4920 = EDGE_CURVE ( 'NONE', #9740, #3225, #8572, .T. ) ;
#4921 = DIRECTION ( 'NONE',  ( 0.000000000000000000, 0.000000000000000000, -1.000000000000000000 ) ) ;
#4922 = CARTESIAN_POINT ( 'NONE',  ( 11.68706106293763369, -3.864370397872626928, 37.20800715665480851 ) ) ;
#4923 = DIRECTION ( 'NONE',  ( 0.000000000000000000, 1.000000000000000000, 0.000000000000000000 ) ) ;
#4924 = CIRCLE ( 'NONE', #7918, 2.500000000000002220 ) ;
#4925 = DIRECTION ( 'NONE',  ( 0.000000000000000000, 0.000000000000000000, 1.000000000000000000 ) ) ;
#4926 = CIRCLE ( 'NONE', #1922, 38.00000000000000711 ) ;
#4927 = LINE ( 'NONE', #7941, #8515 ) ;
#4928 = EDGE_CURVE ( 'NONE', #1931, #3415, #4776, .T. ) ;
#4929 = EDGE_CURVE ( 'NONE', #3340, #5097, #6150, .T. ) ;
#4930 = ORIENTED_EDGE ( 'NONE', *, *, #3946, .T. ) ;
#4931 = LINE ( 'NONE', #7944, #2361 ) ;
#4932 = CARTESIAN_POINT ( 'NONE',  ( 5.562309845534932684, 60.99999999999999289, -28.56426808735048439 ) ) ;
#4933 = EDGE_CURVE ( 'NONE', #7524, #6996, #3327, .T. ) ;
#4934 = ORIENTED_EDGE ( 'NONE', *, *, #2746, .F. ) ;
#4935 = DIRECTION ( 'NONE',  ( -1.820952055660014662E-28, -1.000000000000000000, 6.508102468073347395E-30 ) ) ;
#4936 = LINE ( 'NONE', #2006, #1521 ) ;
#4937 = CARTESIAN_POINT ( 'NONE',  ( -12.40769890286448529, 8.723482751359334486, 36.97414555372668588 ) ) ;
#4938 = LINE ( 'NONE', #4152, #3023 ) ;
#4939 = ADVANCED_FACE ( 'NONE', ( #3434 ), #3140, .T. ) ;
#4940 = VECTOR ( 'NONE', #8262, 1000.000000000000000 ) ;
#4941 = DIRECTION ( 'NONE',  ( 0.000000000000000000, 0.000000000000000000, 1.000000000000000000 ) ) ;
#4942 = VECTOR ( 'NONE', #6941, 1000.000000000000000 ) ;
#4943 = EDGE_LOOP ( 'NONE', ( #8370, #3398, #1347, #3435 ) ) ;
#4944 = DIRECTION ( 'NONE',  ( -0.000000000000000000, -0.000000000000000000, 1.000000000000000000 ) ) ;
#4945 = DIRECTION ( 'NONE',  ( 0.000000000000000000, 1.000000000000000000, 0.000000000000000000 ) ) ;
#4946 = ORIENTED_EDGE ( 'NONE', *, *, #2373, .F. ) ;
#4947 = DIRECTION ( 'NONE',  ( -0.3286710990610907657, 0.000000000000000000, -0.9444444444444440867 ) ) ;
#4948 = PRODUCT_DEFINITION ( 'UNKNOWN', '', #3976, #4901 ) ;
#4949 = FACE_OUTER_BOUND ( 'NONE', #956, .T. ) ;
#4950 = CARTESIAN_POINT ( 'NONE',  ( 5.533140936547730426, 11.68019839214159639, 38.70043871012786241 ) ) ;
#4951 =( LENGTH_UNIT ( ) NAMED_UNIT ( * ) SI_UNIT ( .MILLI., .METRE. ) );
#4952 = VERTEX_POINT ( 'NONE', #378 ) ;
#4953 = CARTESIAN_POINT ( 'NONE',  ( -8.216777476527274970, 78.08723716182652197, -23.61111111111111427 ) ) ;
#4954 = ORIENTED_EDGE ( 'NONE', *, *, #1633, .F. ) ;
#4955 = CARTESIAN_POINT ( 'NONE',  ( 9.860132971832495485, 59.99999999999999289, 28.33333333333341031 ) ) ;
#4956 = ORIENTED_EDGE ( 'NONE', *, *, #7218, .T. ) ;
#4957 = ORIENTED_EDGE ( 'NONE', *, *, #8719, .T. ) ;
#4958 = CARTESIAN_POINT ( 'NONE',  ( -9.727440649738706924, -6.942074567273613717, 37.76869895888170703 ) ) ;
#4959 = VECTOR ( 'NONE', #6585, 1000.000000000000000 ) ;
#4960 = DIRECTION ( 'NONE',  ( -0.000000000000000000, 1.000000000000000000, -0.000000000000000000 ) ) ;
#4961 = CARTESIAN_POINT ( 'NONE',  ( 1.555535097482682654E-26, 78.08723716182652197, -25.00000000000000000 ) ) ;
#4962 = AXIS2_PLACEMENT_3D ( 'NONE', #8582, #4047, #6986 ) ;
#4963 = ORIENTED_EDGE ( 'NONE', *, *, #8365, .T. ) ;
#4964 = DIRECTION ( 'NONE',  ( -1.000000000000000000, -0.000000000000000000, -0.000000000000000000 ) ) ;
#4965 = ORIENTED_EDGE ( 'NONE', *, *, #352, .F. ) ;
#4966 = ORIENTED_EDGE ( 'NONE', *, *, #5797, .T. ) ;
#4967 = LINE ( 'NONE', #6483, #311 ) ;
#4968 = CARTESIAN_POINT ( 'NONE',  ( -30.12488991936162464, 28.28385863652524179, -5.999999999999996447 ) ) ;
#4969 = AXIS2_PLACEMENT_3D ( 'NONE', #2696, #5629, #6407 ) ;
#4970 = DIRECTION ( 'NONE',  ( -0.000000000000000000, 1.000000000000000000, -0.000000000000000000 ) ) ;
#4971 = DIRECTION ( 'NONE',  ( 0.000000000000000000, 0.000000000000000000, 1.000000000000000000 ) ) ;
#4972 = CARTESIAN_POINT ( 'NONE',  ( 9.389914726526274261E-27, 51.50000000000032685, 2.896598636358402723E-28 ) ) ;
#4973 = EDGE_CURVE ( 'NONE', #8688, #742, #2525, .T. ) ;
#4974 = VECTOR ( 'NONE', #2025, 1000.000000000000000 ) ;
#4975 = CIRCLE ( 'NONE', #7334, 37.00000000000000711 ) ;
#4976 = ORIENTED_EDGE ( 'NONE', *, *, #8177, .F. ) ;
#4977 = DIRECTION ( 'NONE',  ( -0.6195972517514870548, 0.000000000000000000, -0.7849198975831892522 ) ) ;
#4978 = PLANE ( 'NONE',  #4489 ) ;
#4979 = VECTOR ( 'NONE', #1147, 1000.000000000000000 ) ;
#4980 = ORIENTED_EDGE ( 'NONE', *, *, #965, .T. ) ;
#4981 = DIRECTION ( 'NONE',  ( -1.000000000000000000, 0.000000000000000000, 1.084202172485503448E-16 ) ) ;
#4982 = DIRECTION ( 'NONE',  ( 1.735493991486225972E-29, -6.508102468073347395E-30, -1.000000000000000000 ) ) ;
#4983 = VECTOR ( 'NONE', #7380, 1000.000000000000000 ) ;
#4984 = CARTESIAN_POINT ( 'NONE',  ( 0.000000000000000000, -10.00000000000000533, 0.000000000000000000 ) ) ;
#4985 = VECTOR ( 'NONE', #522, 1000.000000000000000 ) ;
#4986 = EDGE_CURVE ( 'NONE', #915, #9635, #487, .T. ) ;
#4987 = EDGE_CURVE ( 'NONE', #880, #6509, #8043, .T. ) ;
#4988 = LINE ( 'NONE', #724, #3669 ) ;
#4989 = ADVANCED_FACE ( 'NONE', ( #3377 ), #6387, .T. ) ;
#4990 = VECTOR ( 'NONE', #8526, 1000.000000000000000 ) ;
#4991 = FACE_BOUND ( 'NONE', #1613, .T. ) ;
#4992 = DIRECTION ( 'NONE',  ( 0.000000000000000000, 0.000000000000000000, 1.000000000000000000 ) ) ;
#4993 = ORIENTED_EDGE ( 'NONE', *, *, #710, .F. ) ;
#4994 = DIRECTION ( 'NONE',  ( -1.735493991486225972E-29, 6.508102468073347395E-30, 1.000000000000000000 ) ) ;
#4995 = CARTESIAN_POINT ( 'NONE',  ( -9.151040477096435311, -15.00000000000093614, 37.02450192303366094 ) ) ;
#4996 = ORIENTED_EDGE ( 'NONE', *, *, #4929, .T. ) ;
#4997 = AXIS2_PLACEMENT_3D ( 'NONE', #1380, #4945, #2654 ) ;
#4998 = EDGE_CURVE ( 'NONE', #8477, #5016, #3186, .T. ) ;
#4999 = DIRECTION ( 'NONE',  ( 0.000000000000000000, -0.8660254037844385966, -0.5000000000000003331 ) ) ;
#5000 = DIRECTION ( 'NONE',  ( 0.000000000000000000, -1.000000000000000000, 0.000000000000000000 ) ) ;
#5001 = ADVANCED_FACE ( 'NONE', ( #2484 ), #246, .F. ) ;
#5002 = CARTESIAN_POINT ( 'NONE',  ( 7.533895508403737118, 9.914173740682880265, 38.39536267294633376 ) ) ;
#5003 = VERTEX_POINT ( 'NONE', #4689 ) ;
#5004 = CARTESIAN_POINT ( 'NONE',  ( -33.06426808735054124, 59.99576382555915899, -3.062309845534580077 ) ) ;
#5005 = VERTEX_POINT ( 'NONE', #5327 ) ;
#5006 = CARTESIAN_POINT ( 'NONE',  ( 35.54742948121823787, 59.05243086228237104, 5.228649803729175538 ) ) ;
#5007 = ORIENTED_EDGE ( 'NONE', *, *, #7272, .T. ) ;
#5008 = VECTOR ( 'NONE', #8183, 1000.000000000000000 ) ;
#5009 = ORIENTED_EDGE ( 'NONE', *, *, #255, .F. ) ;
#5010 = CARTESIAN_POINT ( 'NONE',  ( -5.485052425114111507, 16.96760966600532683, 38.61446893340349362 ) ) ;
#5011 = FACE_OUTER_BOUND ( 'NONE', #4656, .T. ) ;
#5012 = DIRECTION ( 'NONE',  ( -1.000000000000000000, -0.000000000000000000, -0.000000000000000000 ) ) ;
#5013 = EDGE_CURVE ( 'NONE', #6355, #6584, #780, .T. ) ;
#5014 = ORIENTED_EDGE ( 'NONE', *, *, #4720, .F. ) ;
#5015 = CARTESIAN_POINT ( 'NONE',  ( 1.300000000000000044, 0.7216878364870328300, 1.250000000000000000 ) ) ;
#5016 = VERTEX_POINT ( 'NONE', #8485 ) ;
#5017 = LINE ( 'NONE', #8123, #1799 ) ;
#5018 = LINE ( 'NONE', #5115, #8830 ) ;
#5019 = PLANE ( 'NONE',  #4129 ) ;
#5020 = DIRECTION ( 'NONE',  ( 0.000000000000000000, 1.000000000000000000, 0.000000000000000000 ) ) ;
#5021 = CARTESIAN_POINT ( 'NONE',  ( 29.00000000000000355, 28.99999999999997158, -4.000000000000007105 ) ) ;
#5022 = EDGE_LOOP ( 'NONE', ( #3266, #7088, #5312, #4739 ) ) ;
#5023 = PLANE ( 'NONE',  #6695 ) ;
#5024 = CARTESIAN_POINT ( 'NONE',  ( 0.3492264405225555812, 13.29422555222517843, 43.99967941412595707 ) ) ;
#5025 = ORIENTED_EDGE ( 'NONE', *, *, #1233, .T. ) ;
#5026 = LINE ( 'NONE', #1229, #8228 ) ;
#5027 = CARTESIAN_POINT ( 'NONE',  ( 12.20000000000000107, 0.000000000000000000, 0.000000000000000000 ) ) ;
#5028 = DIRECTION ( 'NONE',  ( -0.9444444444444315412, 0.000000000000000000, 0.3286710990611268479 ) ) ;
#5029 = DIRECTION ( 'NONE',  ( 0.000000000000000000, 0.000000000000000000, -1.000000000000000000 ) ) ;
#5030 = EDGE_CURVE ( 'NONE', #1752, #1969, #3635, .T. ) ;
#5031 = FACE_OUTER_BOUND ( 'NONE', #8083, .T. ) ;
#5032 = CARTESIAN_POINT ( 'NONE',  ( 1.555535097482682654E-26, 78.08723716182652197, -25.00000000000000000 ) ) ;
#5033 = ADVANCED_FACE ( 'NONE', ( #3939 ), #9131, .F. ) ;
#5034 = ORIENTED_EDGE ( 'NONE', *, *, #4068, .F. ) ;
#5035 = FACE_BOUND ( 'NONE', #7965, .T. ) ;
#5036 = CARTESIAN_POINT ( 'NONE',  ( -9.491181639781968826, -6.034149515792501361, 37.89378918816769470 ) ) ;
#5037 = EDGE_CURVE ( 'NONE', #4366, #4234, #6250, .T. ) ;
#5038 = ORIENTED_EDGE ( 'NONE', *, *, #9033, .T. ) ;
#5039 = CARTESIAN_POINT ( 'NONE',  ( 33.06426808735054124, 49.99999999999999289, 8.062309845534588959 ) ) ;
#5040 = ADVANCED_FACE ( 'NONE', ( #2395 ), #5479, .T. ) ;
#5041 = AXIS2_PLACEMENT_3D ( 'NONE', #2681, #8076, #5706 ) ;
#5042 = CARTESIAN_POINT ( 'NONE',  ( 1.040310318760209318E-26, 55.00000000000030553, -26.00000000000003197 ) ) ;
#5043 = DIRECTION ( 'NONE',  ( 1.735493991486225972E-29, -6.508102468073347395E-30, -1.000000000000000000 ) ) ;
#5044 = CARTESIAN_POINT ( 'NONE',  ( 33.06426808735054124, 63.19999999999999574, 5.562309845534584518 ) ) ;
#5045 = ADVANCED_FACE ( 'NONE', ( #7551 ), #8694, .T. ) ;
#5046 = ORIENTED_EDGE ( 'NONE', *, *, #5581, .F. ) ;
#5047 = DIRECTION ( 'NONE',  ( -0.9860132971832694659, -1.788557213313974350E-28, 0.1666666666666658247 ) ) ;
#5048 = ADVANCED_FACE ( 'NONE', ( #9080 ), #2297, .T. ) ;
#5049 = VERTEX_POINT ( 'NONE', #7597 ) ;
#5050 = CARTESIAN_POINT ( 'NONE',  ( -2.094888803305880518E-13, 59.99999999999999289, 30.00000000000000711 ) ) ;
#5051 = EDGE_CURVE ( 'NONE', #3045, #2848, #8385, .T. ) ;
#5052 = VERTEX_POINT ( 'NONE', #6982 ) ;
#5053 = DIRECTION ( 'NONE',  ( -1.820952055660014662E-28, -1.000000000000000000, -7.038118388768679669E-30 ) ) ;
#5054 = VECTOR ( 'NONE', #921, 1000.000000000000000 ) ;
#5055 = ORIENTED_EDGE ( 'NONE', *, *, #930, .T. ) ;
#5056 = EDGE_CURVE ( 'NONE', #269, #2192, #1904, .T. ) ;
#5057 = CARTESIAN_POINT ( 'NONE',  ( -7.036077784066177010, 10.44445367756955534, 38.48139619194807182 ) ) ;
#5058 = DIRECTION ( 'NONE',  ( 0.000000000000000000, 0.000000000000000000, -1.000000000000000000 ) ) ;
#5059 = CARTESIAN_POINT ( 'NONE',  ( 0.000000000000000000, -4.999999999999999112, 0.000000000000000000 ) ) ;
#5060 = AXIS2_PLACEMENT_3D ( 'NONE', #9655, #5020, #670 ) ;
#5061 = EDGE_LOOP ( 'NONE', ( #7097, #4916, #9257, #4877 ) ) ;
#5062 = CARTESIAN_POINT ( 'NONE',  ( 0.000000000000000000, 39.99999999999999289, 0.000000000000000000 ) ) ;
#5063 = ORIENTED_EDGE ( 'NONE', *, *, #7149, .F. ) ;
#5064 = CARTESIAN_POINT ( 'NONE',  ( 9.661664702339496822E-27, 53.00000000000031974, 2.823413298471687761E-28 ) ) ;
#5065 = CARTESIAN_POINT ( 'NONE',  ( -5.562309845534584518, 59.99999999999999289, 35.56426808735054834 ) ) ;
#5066 = AXIS2_PLACEMENT_3D ( 'NONE', #6288, #7846, #7079 ) ;
#5067 = CARTESIAN_POINT ( 'NONE',  ( 0.000000000000000000, 3.294852476641296768, 300.0000000000000000 ) ) ;
#5068 = CARTESIAN_POINT ( 'NONE',  ( 2.021687836487040535, 0.000000000000000000, 2.168404344971008868E-16 ) ) ;
#5069 = CARTESIAN_POINT ( 'NONE',  ( -8.216777476527294510, 54.50000000000031264, -23.61111111111111427 ) ) ;
#5070 = EDGE_CURVE ( 'NONE', #2338, #9259, #2511, .T. ) ;
#5071 = VECTOR ( 'NONE', #3786, 1000.000000000000000 ) ;
#5072 = DIRECTION ( 'NONE',  ( 0.000000000000000000, 0.5000000000000001110, 0.8660254037844385966 ) ) ;
#5073 = VERTEX_POINT ( 'NONE', #4590 ) ;
#5074 = FACE_OUTER_BOUND ( 'NONE', #8522, .T. ) ;
#5075 = CARTESIAN_POINT ( 'NONE',  ( 9.866687305369380212, 4.955150770795770931, 41.43633485533133864 ) ) ;
#5076 = ORIENTED_EDGE ( 'NONE', *, *, #2329, .F. ) ;
#5077 = CARTESIAN_POINT ( 'NONE',  ( 5.137569555611264605, 60.99999999999999289, 32.59762842694627949 ) ) ;
#5078 = CARTESIAN_POINT ( 'NONE',  ( -6.000000000000005329, 30.00000000000000000, -26.32489316217636954 ) ) ;
#5079 = CARTESIAN_POINT ( 'NONE',  ( 0.000000000000000000, 30.00000000000000000, 0.000000000000000000 ) ) ;
#5080 = CARTESIAN_POINT ( 'NONE',  ( 4.000000000000001776, 30.00000000000000000, 0.000000000000000000 ) ) ;
#5081 = VECTOR ( 'NONE', #6898, 1000.000000000000000 ) ;
#5082 = FACE_BOUND ( 'NONE', #6965, .T. ) ;
#5083 = DIRECTION ( 'NONE',  ( 0.000000000000000000, 1.000000000000000000, 0.000000000000000000 ) ) ;
#5084 = EDGE_LOOP ( 'NONE', ( #7313, #6338, #1053, #3798 ) ) ;
#5085 = DIRECTION ( 'NONE',  ( -0.000000000000000000, -1.000000000000000000, -0.000000000000000000 ) ) ;
#5086 = CARTESIAN_POINT ( 'NONE',  ( -4.487157684392466095, -15.00000000000000000, 29.19769096421646282 ) ) ;
#5087 = EDGE_CURVE ( 'NONE', #6014, #4753, #835, .T. ) ;
#5088 = CIRCLE ( 'NONE', #9353, 27.99999999999999289 ) ;
#5089 = ORIENTED_EDGE ( 'NONE', *, *, #2519, .T. ) ;
#5090 = FACE_OUTER_BOUND ( 'NONE', #338, .T. ) ;
#5091 = CARTESIAN_POINT ( 'NONE',  ( 25.90235662024527485, 59.99999999999999289, -20.44670930779904339 ) ) ;
#5092 = ORIENTED_EDGE ( 'NONE', *, *, #4564, .T. ) ;
#5093 = VECTOR ( 'NONE', #4030, 1000.000000000000114 ) ;
#5094 = VECTOR ( 'NONE', #5384, 1000.000000000000000 ) ;
#5095 = CARTESIAN_POINT ( 'NONE',  ( 6.062272466284918337, 11.31083119101153578, 38.63159523596766576 ) ) ;
#5096 = CARTESIAN_POINT ( 'NONE',  ( 0.000000000000000000, 0.000000000000000000, 0.000000000000000000 ) ) ;
#5097 = VERTEX_POINT ( 'NONE', #3088 ) ;
#5098 = CARTESIAN_POINT ( 'NONE',  ( -34.60286690457041914, 59.67177527313210561, -3.585274540811277610 ) ) ;
#5099 = ORIENTED_EDGE ( 'NONE', *, *, #4451, .T. ) ;
#5100 = CARTESIAN_POINT ( 'NONE',  ( 35.21620900558183820, 59.09151583898437821, 6.845072491844678808 ) ) ;
#5101 = ORIENTED_EDGE ( 'NONE', *, *, #201, .F. ) ;
#5102 = DIRECTION ( 'NONE',  ( 0.000000000000000000, 0.000000000000000000, 1.000000000000000000 ) ) ;
#5103 = B_SPLINE_CURVE_WITH_KNOTS ( 'NONE', 3,
 ( #5452, #1695, #3116, #8411, #4664, #7575, #4711, #3014 ),
 .UNSPECIFIED., .F., .F.,
 ( 4, 2, 2, 4 ),
 ( 0.007099638519839682714, 0.008372149287075627763, 0.009008404670693602456, 0.009644660054311575414 ),
 .UNSPECIFIED. ) ;
#5104 = VERTEX_POINT ( 'NONE', #6888 ) ;
#5105 = CARTESIAN_POINT ( 'NONE',  ( -7.729170831334030822, 9.683805115199277225, 38.35949281304758074 ) ) ;
#5106 = CARTESIAN_POINT ( 'NONE',  ( -5.562309845534584518, 49.99999999999999289, 33.06426808735054124 ) ) ;
#5107 = DIRECTION ( 'NONE',  ( 0.000000000000000000, 0.000000000000000000, 1.000000000000000000 ) ) ;
#5108 = EDGE_CURVE ( 'NONE', #5461, #8444, #6103, .T. ) ;
#5109 = ADVANCED_FACE ( 'NONE', ( #4643 ), #7641, .T. ) ;
#5110 = ADVANCED_FACE ( 'NONE', ( #5616 ), #5756, .F. ) ;
#5111 = VERTEX_POINT ( 'NONE', #7080 ) ;
#5112 = DIRECTION ( 'NONE',  ( -0.000000000000000000, -1.000000000000000000, -0.000000000000000000 ) ) ;
#5113 = ORIENTED_EDGE ( 'NONE', *, *, #396, .T. ) ;
#5114 = CARTESIAN_POINT ( 'NONE',  ( 8.106083942516887559E-27, 44.50000000000019185, 2.954376534690019799E-28 ) ) ;
#5115 = CARTESIAN_POINT ( 'NONE',  ( -30.00000000000001066, 39.99999999999999289, -3.142333204958820777E-13 ) ) ;
#5116 = DIRECTION ( 'NONE',  ( 0.000000000000000000, 1.000000000000000000, 0.000000000000000000 ) ) ;
#5117 = CARTESIAN_POINT ( 'NONE',  ( 27.56211685706808723, 60.99999999999999289, 15.25056439471416780 ) ) ;
#5118 = AXIS2_PLACEMENT_3D ( 'NONE', #6444, #9474, #2692 ) ;
#5119 =( REPRESENTATION_RELATIONSHIP ('NONE','NONE', #5841, #2928 ) REPRESENTATION_RELATIONSHIP_WITH_TRANSFORMATION ( #852 )SHAPE_REPRESENTATION_RELATIONSHIP( ) );
#5120 = EDGE_CURVE ( 'NONE', #8580, #3849, #2675, .T. ) ;
#5121 = DIRECTION ( 'NONE',  ( -0.000000000000000000, -1.000000000000000000, -0.000000000000000000 ) ) ;
#5122 = VECTOR ( 'NONE', #3136, 1000.000000000000000 ) ;
#5123 = EDGE_LOOP ( 'NONE', ( #4548, #7216, #8386, #394 ) ) ;
#5124 = AXIS2_PLACEMENT_3D ( 'NONE', #6313, #5083, #7204 ) ;
#5125 = CARTESIAN_POINT ( 'NONE',  ( -18.58791755254457456, 39.99999999999999289, -23.54759692749571443 ) ) ;
#5126 = CARTESIAN_POINT ( 'NONE',  ( 1.097009696322969542E-26, 52.00000000000031974, -25.00000000000000000 ) ) ;
#5127 = DIRECTION ( 'NONE',  ( 0.000000000000000000, -1.000000000000000000, 0.000000000000000000 ) ) ;
#5128 = CARTESIAN_POINT ( 'NONE',  ( -5.999999999999998224, 30.00000000000000000, 26.32489316217636954 ) ) ;
#5129 = DIRECTION ( 'NONE',  ( -0.3271946967961527619, -0.000000000000000000, 0.9449569463147374782 ) ) ;
#5130 = DIRECTION ( 'NONE',  ( 1.000000000000000000, 0.000000000000000000, 0.000000000000000000 ) ) ;
#5131 = AXIS2_PLACEMENT_3D ( 'NONE', #6413, #2503, #5539 ) ;
#5132 = CIRCLE ( 'NONE', #1657, 28.99999999999995026 ) ;
#5133 = PLANE ( 'NONE',  #319 ) ;
#5134 = VECTOR ( 'NONE', #7562, 1000.000000000000000 ) ;
#5135 = CIRCLE ( 'NONE', #5459, 26.00000000000015987 ) ;
#5136 = PLANE ( 'NONE',  #9697 ) ;
#5137 = AXIS2_PLACEMENT_3D ( 'NONE', #2666, #4766, #428 ) ;
#5138 = EDGE_CURVE ( 'NONE', #8953, #2569, #7905, .T. ) ;
#5139 = ORIENTED_EDGE ( 'NONE', *, *, #7055, .F. ) ;
#5140 = PLANE ( 'NONE',  #9383 ) ;
#5141 = CARTESIAN_POINT ( 'NONE',  ( -5.832239843001731927, -15.00000000000000000, 28.64283837909960795 ) ) ;
#5142 = ORIENTED_EDGE ( 'NONE', *, *, #2923, .T. ) ;
#5143 = LINE ( 'NONE', #8195, #1293 ) ;
#5144 = AXIS2_PLACEMENT_3D ( 'NONE', #1036, #6995, #2548 ) ;
#5145 = AXIS2_PLACEMENT_3D ( 'NONE', #6809, #2205, #3006 ) ;
#5146 = CARTESIAN_POINT ( 'NONE',  ( 0.000000000000000000, 38.99999999999993605, 0.000000000000000000 ) ) ;
#5147 = VERTEX_POINT ( 'NONE', #3281 ) ;
#5148 = CARTESIAN_POINT ( 'NONE',  ( 1.772214115361161912, 18.16925905107996186, 38.96216795829242585 ) ) ;
#5149 = APPLICATION_PROTOCOL_DEFINITION ( 'draft international standard', 'automotive_design', 1998, #3733 ) ;
#5150 = ORIENTED_EDGE ( 'NONE', *, *, #8819, .T. ) ;
#5151 = CARTESIAN_POINT ( 'NONE',  ( -33.23540996127940872, 59.98874451312625666, -3.062309845534580077 ) ) ;
#5152 = VECTOR ( 'NONE', #5627, 1000.000000000000000 ) ;
#5153 = VERTEX_POINT ( 'NONE', #2683 ) ;
#5154 = CYLINDRICAL_SURFACE ( 'NONE', #6222, 38.00000000000000711 ) ;
#5155 = ORIENTED_EDGE ( 'NONE', *, *, #2926, .T. ) ;
#5156 = CARTESIAN_POINT ( 'NONE',  ( 15.25056439471407188, 60.99999999999999289, -27.56211685706813341 ) ) ;
#5157 = ORIENTED_EDGE ( 'NONE', *, *, #7514, .F. ) ;
#5158 = CARTESIAN_POINT ( 'NONE',  ( -1.624225145205289156, 13.16760741291165537, 43.93520348923563290 ) ) ;
#5159 = DIRECTION ( 'NONE',  ( 0.000000000000000000, 1.000000000000000000, 0.000000000000000000 ) ) ;
#5160 = FACE_OUTER_BOUND ( 'NONE', #1943, .T. ) ;
#5161 = VECTOR ( 'NONE', #3742, 1000.000000000000000 ) ;
#5162 = ORIENTED_EDGE ( 'NONE', *, *, #5762, .F. ) ;
#5163 = DIRECTION ( 'NONE',  ( 0.000000000000000000, 0.000000000000000000, -1.000000000000000000 ) ) ;
#5164 = VERTEX_POINT ( 'NONE', #6487 ) ;
#5165 = VERTEX_POINT ( 'NONE', #291 ) ;
#5166 = EDGE_CURVE ( 'NONE', #9301, #300, #9512, .T. ) ;
#5167 = CARTESIAN_POINT ( 'NONE',  ( -2.304377683636469277E-13, 54.99999999999999289, 33.00000000000000711 ) ) ;
#5168 = DIRECTION ( 'NONE',  ( 1.000000000000000000, 0.000000000000000000, 0.000000000000000000 ) ) ;
#5169 = CARTESIAN_POINT ( 'NONE',  ( 0.000000000000000000, 61.99999999999999289, 0.000000000000000000 ) ) ;
#5170 = EDGE_CURVE ( 'NONE', #9011, #2376, #5842, .T. ) ;
#5171 = CARTESIAN_POINT ( 'NONE',  ( 9.922629470464150863E-27, 54.50000000000031264, 2.962080254467568742E-28 ) ) ;
#5172 = EDGE_CURVE ( 'NONE', #4095, #4849, #384, .T. ) ;
#5173 = CARTESIAN_POINT ( 'NONE',  ( 23.54759692749571087, 39.99999999999999289, -18.58791755254458167 ) ) ;
#5174 = CARTESIAN_POINT ( 'NONE',  ( 0.000000000000000000, 59.99999999999999289, -30.00000000000000711 ) ) ;
#5175 = LINE ( 'NONE', #9473, #5008 ) ;
#5176 = FACE_OUTER_BOUND ( 'NONE', #359, .T. ) ;
#5177 = ADVANCED_FACE ( 'NONE', ( #5708 ), #6395, .F. ) ;
#5178 = CARTESIAN_POINT ( 'NONE',  ( 0.000000000000000000, 39.99999999999999289, 0.000000000000000000 ) ) ;
#5179 = CARTESIAN_POINT ( 'NONE',  ( 31.18357922838634266, 54.99999999999999289, 10.79742499427304381 ) ) ;
#5180 = EDGE_CURVE ( 'NONE', #4125, #2236, #6439, .T. ) ;
#5181 = CARTESIAN_POINT ( 'NONE',  ( 0.000000000000000000, 0.000000000000000000, -38.00000000000000711 ) ) ;
#5182 = CARTESIAN_POINT ( 'NONE',  ( 0.000000000000000000, 30.00000000000000000, 0.000000000000000000 ) ) ;
#5183 = ORIENTED_EDGE ( 'NONE', *, *, #5947, .F. ) ;
#5184 = DIRECTION ( 'NONE',  ( -0.3286710990610922090, -6.289316826390952918E-29, -0.9444444444444435316 ) ) ;
#5185 = CARTESIAN_POINT ( 'NONE',  ( 2.108145055611895469, -9.304652320644109409, 39.45342799411329793 ) ) ;
#5186 = ORIENTED_EDGE ( 'NONE', *, *, #1811, .T. ) ;
#5187 = DIRECTION ( 'NONE',  ( 0.000000000000000000, 0.000000000000000000, -1.000000000000000000 ) ) ;
#5188 = LINE ( 'NONE', #2199, #1506 ) ;
#5189 = FACE_OUTER_BOUND ( 'NONE', #8033, .T. ) ;
#5190 = ORIENTED_EDGE ( 'NONE', *, *, #526, .T. ) ;
#5191 = ADVANCED_FACE ( 'NONE', ( #2585 ), #6936, .F. ) ;
#5192 = CARTESIAN_POINT ( 'NONE',  ( 10.54343430594074960, -5.895781167747204954, 37.55119601223130843 ) ) ;
#5193 = SHAPE_DEFINITION_REPRESENTATION ( #4578, #1483 ) ;
#5194 = VERTEX_POINT ( 'NONE', #3337 ) ;
#5195 = LINE ( 'NONE', #4555, #887 ) ;
#5196 = ORIENTED_EDGE ( 'NONE', *, *, #991, .T. ) ;
#5197 = FACE_OUTER_BOUND ( 'NONE', #9541, .T. ) ;
#5198 = ORIENTED_EDGE ( 'NONE', *, *, #8614, .F. ) ;
#5199 = CARTESIAN_POINT ( 'NONE',  ( -12.16083066526040213, 60.00000000000029843, -34.94444444444452103 ) ) ;
#5200 = ORIENTED_EDGE ( 'NONE', *, *, #7223, .T. ) ;
#5201 = CIRCLE ( 'NONE', #6448, 2.500000000000002220 ) ;
#5202 = DIRECTION ( 'NONE',  ( -0.000000000000000000, 0.000000000000000000, 1.000000000000000000 ) ) ;
#5203 = CARTESIAN_POINT ( 'NONE',  ( 9.417027056075828427E-27, 44.50000000000019185, -25.00000000000000000 ) ) ;
#5204 = AXIS2_PLACEMENT_3D ( 'NONE', #7028, #6283, #9310 ) ;
#5205 = VERTEX_POINT ( 'NONE', #2638 ) ;
#5206 = DIRECTION ( 'NONE',  ( 0.000000000000000000, 0.000000000000000000, -1.000000000000000000 ) ) ;
#5207 = LINE ( 'NONE', #6480, #4486 ) ;
#5208 = VERTEX_POINT ( 'NONE', #1756 ) ;
#5209 = DIRECTION ( 'NONE',  ( 0.000000000000000000, 1.000000000000000000, 0.000000000000000000 ) ) ;
#5210 = FACE_OUTER_BOUND ( 'NONE', #4196, .T. ) ;
#5211 = EDGE_CURVE ( 'NONE', #7361, #849, #1740, .T. ) ;
#5212 = CYLINDRICAL_SURFACE ( 'NONE', #8446, 1.499999999999999556 ) ;
#5213 = SHAPE_REPRESENTATION ( 'Lever with a Die for Securing the Metal Body', ( #6314 ), #2196 ) ;
#5214 = VECTOR ( 'NONE', #1903, 1000.000000000000000 ) ;
#5215 = EDGE_CURVE ( 'NONE', #8835, #5097, #2532, .T. ) ;
#5216 = ADVANCED_FACE ( 'NONE', ( #8578 ), #1806, .T. ) ;
#5217 = CARTESIAN_POINT ( 'NONE',  ( 0.000000000000000000, 54.99999999999999289, 0.000000000000000000 ) ) ;
#5218 = ORIENTED_EDGE ( 'NONE', *, *, #9565, .F. ) ;
#5219 = CARTESIAN_POINT ( 'NONE',  ( -0.01963426291156584666, -6.705128248126137613, 43.99999014335539016 ) ) ;
#5220 = AXIS2_PLACEMENT_3D ( 'NONE', #6587, #5116, #1362 ) ;
#5221 = DIRECTION ( 'NONE',  ( -1.820952055660014662E-28, -1.000000000000000000, -7.038118388768679669E-30 ) ) ;
#5222 = FACE_OUTER_BOUND ( 'NONE', #4280, .T. ) ;
#5223 = DIRECTION ( 'NONE',  ( -1.820952055660014662E-28, -1.000000000000000000, -7.038118388768679669E-30 ) ) ;
#5224 = CARTESIAN_POINT ( 'NONE',  ( -0.6447393712377219588, 18.29485247664131364, 39.00000000000001421 ) ) ;
#5225 = EDGE_CURVE ( 'NONE', #4748, #5814, #4089, .T. ) ;
#5226 = EDGE_CURVE ( 'NONE', #2408, #742, #1594, .T. ) ;
#5227 = EDGE_CURVE ( 'NONE', #9622, #9126, #4139, .T. ) ;
#5228 = FACE_OUTER_BOUND ( 'NONE', #5450, .T. ) ;
#5229 = CARTESIAN_POINT ( 'NONE',  ( -31.00000000000000711, 27.42469319230600533, 6.000000000000009770 ) ) ;
#5230 = VERTEX_POINT ( 'NONE', #7135 ) ;
#5231 = DIRECTION ( 'NONE',  ( 0.5773502691896205130, 0.5773502691896365002, -0.5773502691896204020 ) ) ;
#5232 = CARTESIAN_POINT ( 'NONE',  ( 1.153709073885729765E-26, 55.00000000000030553, -37.00000000000000711 ) ) ;
#5233 = ORIENTED_EDGE ( 'NONE', *, *, #790, .F. ) ;
#5234 = AXIS2_PLACEMENT_3D ( 'NONE', #5077, #8087, #7350 ) ;
#5235 = DIRECTION ( 'NONE',  ( -0.9860132971832693549, -1.788557213313974126E-28, 0.1666666666666657970 ) ) ;
#5236 = LINE ( 'NONE', #648, #8921 ) ;
#5237 = CYLINDRICAL_SURFACE ( 'NONE', #3302, 26.00000000000008171 ) ;
#5238 = CARTESIAN_POINT ( 'NONE',  ( 8.737909304966237301, 8.199549718101609486, 38.15650413348530634 ) ) ;
#5239 = APPLICATION_PROTOCOL_DEFINITION ( 'draft international standard', 'automotive_design', 1998, #3089 ) ;
#5240 = AXIS2_PLACEMENT_3D ( 'NONE', #4899, #1738, #6270 ) ;
#5241 = ORIENTED_EDGE ( 'NONE', *, *, #5120, .F. ) ;
#5242 = CARTESIAN_POINT ( 'NONE',  ( -33.06426808735054124, 60.99999999999999289, -1.062309845534581632 ) ) ;
#5243 = FACE_OUTER_BOUND ( 'NONE', #2804, .T. ) ;
#5244 = DIRECTION ( 'NONE',  ( -0.9860132971832693549, -1.788449361237088441E-28, 0.1666666666666662133 ) ) ;
#5245 = ORIENTED_EDGE ( 'NONE', *, *, #4088, .T. ) ;
#5246 = CARTESIAN_POINT ( 'NONE',  ( -33.06426808735054124, 49.99999999999999289, -5.562309845534581854 ) ) ;
#5247 = ORIENTED_EDGE ( 'NONE', *, *, #3689, .F. ) ;
#5248 = LINE ( 'NONE', #8259, #4809 ) ;
#5249 = CARTESIAN_POINT ( 'NONE',  ( 2.200000000000000622, 1.999999999999999112, 0.000000000000000000 ) ) ;
#5250 = VECTOR ( 'NONE', #3884, 1000.000000000000000 ) ;
#5251 = LINE ( 'NONE', #6579, #4940 ) ;
#5252 = AXIS2_PLACEMENT_3D ( 'NONE', #9234, #1763, #342 ) ;
#5253 = ORIENTED_EDGE ( 'NONE', *, *, #8476, .F. ) ;
#5254 = CARTESIAN_POINT ( 'NONE',  ( -5.562309845551829390, 59.00253480853272947, 35.56426808735054834 ) ) ;
#5255 = DIRECTION ( 'NONE',  ( 0.3286710990610922090, 6.289316826390952918E-29, 0.9444444444444435316 ) ) ;
#5256 = AXIS2_PLACEMENT_3D ( 'NONE', #1445, #1354, #4469 ) ;
#5257 = UNCERTAINTY_MEASURE_WITH_UNIT (LENGTH_MEASURE( 1.000000000000000082E-05 ), #7163, 'distance_accuracy_value', 'NONE');
#5258 = ORIENTED_EDGE ( 'NONE', *, *, #8730, .T. ) ;
#5259 = CARTESIAN_POINT ( 'NONE',  ( -6.000000000000005329, -15.00000000000000000, -31.00000000000000711 ) ) ;
#5260 = CARTESIAN_POINT ( 'NONE',  ( 30.00000000000000711, 59.99999999999999289, 1.047444401652940259E-13 ) ) ;
#5261 = VECTOR ( 'NONE', #6533, 1000.000000000000000 ) ;
#5262 = FACE_OUTER_BOUND ( 'NONE', #7050, .T. ) ;
#5263 = CARTESIAN_POINT ( 'NONE',  ( 23.54759692749571443, 39.99999999999999289, -18.58791755254457811 ) ) ;
#5264 = ORIENTED_EDGE ( 'NONE', *, *, #5522, .F. ) ;
#5265 = CARTESIAN_POINT ( 'NONE',  ( 0.000000000000000000, 39.99999999999999289, 0.000000000000000000 ) ) ;
#5266 = CARTESIAN_POINT ( 'NONE',  ( 10.00000000000001599, 3.294852476638864491, 41.36423575989288537 ) ) ;
#5267 = DIRECTION ( 'NONE',  ( 0.000000000000000000, 1.000000000000000000, 0.000000000000000000 ) ) ;
#5268 = CARTESIAN_POINT ( 'NONE',  ( -0.3732932347937627515, -15.00000000000000000, 30.58137713278830105 ) ) ;
#5269 = FACE_OUTER_BOUND ( 'NONE', #8013, .T. ) ;
#5270 = ORIENTED_EDGE ( 'NONE', *, *, #5485, .F. ) ;
#5271 = ADVANCED_FACE ( 'NONE', ( #3386 ), #1451, .F. ) ;
#5272 = CARTESIAN_POINT ( 'NONE',  ( -4.000000000000005329, 30.00000000000000000, -29.00000000000000355 ) ) ;
#5273 = ADVANCED_FACE ( 'NONE', ( #1316 ), #3529, .T. ) ;
#5274 = VECTOR ( 'NONE', #7539, 1000.000000000000000 ) ;
#5275 = TOROIDAL_SURFACE ( 'NONE', #245, 37.00000000000000711, 1.000000000000000888 ) ;
#5276 = DIRECTION ( 'NONE',  ( 0.000000000000000000, 1.000000000000000000, 0.000000000000000000 ) ) ;
#5277 = ORIENTED_EDGE ( 'NONE', *, *, #1848, .F. ) ;
#5278 = DIRECTION ( 'NONE',  ( -1.000000000000000000, -0.000000000000000000, -0.000000000000000000 ) ) ;
#5279 = CARTESIAN_POINT ( 'NONE',  ( 3.456999781945461425, -9.004789367952092505, 39.31782667389276043 ) ) ;
#5280 = ORIENTED_EDGE ( 'NONE', *, *, #9403, .T. ) ;
#5281 = ADVANCED_FACE ( 'NONE', ( #9607, #5210 ), #2175, .T. ) ;
#5282 = EDGE_CURVE ( 'NONE', #2645, #7767, #8049, .T. ) ;
#5283 = VECTOR ( 'NONE', #2787, 1000.000000000000114 ) ;
#5284 = EDGE_CURVE ( 'NONE', #8065, #3045, #7480, .T. ) ;
#5285 = DIRECTION ( 'NONE',  ( 0.000000000000000000, 0.000000000000000000, -1.000000000000000000 ) ) ;
#5286 = DIRECTION ( 'NONE',  ( -0.000000000000000000, -1.000000000000000000, -0.000000000000000000 ) ) ;
#5287 = EDGE_LOOP ( 'NONE', ( #8534, #2287, #2455, #1209 ) ) ;
#5288 = AXIS2_PLACEMENT_3D ( 'NONE', #2715, #2812, #1248 ) ;
#5289 = CARTESIAN_POINT ( 'NONE',  ( 9.900265737266146004, 4.761116128428549921, 37.88407853222265231 ) ) ;
#5290 = CIRCLE ( 'NONE', #2754, 2.500000000000002220 ) ;
#5291 =( NAMED_UNIT ( * ) SI_UNIT ( $, .STERADIAN. ) SOLID_ANGLE_UNIT ( ) );
#5292 = AXIS2_PLACEMENT_3D ( 'NONE', #4027, #4820, #8624 ) ;
#5293 = ORIENTED_EDGE ( 'NONE', *, *, #5138, .T. ) ;
#5294 = VERTEX_POINT ( 'NONE', #7282 ) ;
#5295 = DIRECTION ( 'NONE',  ( -1.820952055660014662E-28, -1.000000000000000000, 6.508102468073347395E-30 ) ) ;
#5296 = DIRECTION ( 'NONE',  ( -0.000000000000000000, -1.000000000000000000, -0.000000000000000000 ) ) ;
#5297 = CARTESIAN_POINT ( 'NONE',  ( -31.00000000000000711, -15.00000000000000000, 6.000000000000009770 ) ) ;
#5298 = ORIENTED_EDGE ( 'NONE', *, *, #5108, .F. ) ;
#5299 = DIRECTION ( 'NONE',  ( 0.9860132971832693549, 1.788557213313974126E-28, -0.1666666666666657970 ) ) ;
#5300 = ORIENTED_EDGE ( 'NONE', *, *, #2477, .F. ) ;
#5301 = EDGE_CURVE ( 'NONE', #7014, #5814, #9317, .T. ) ;
#5302 = AXIS2_PLACEMENT_3D ( 'NONE', #4167, #461, #6460 ) ;
#5303 = FACE_OUTER_BOUND ( 'NONE', #1493, .T. ) ;
#5304 = AXIS2_PLACEMENT_3D ( 'NONE', #1098, #2566, #1881 ) ;
#5305 = ADVANCED_FACE ( 'NONE', ( #2041 ), #5807, .F. ) ;
#5306 = FACE_OUTER_BOUND ( 'NONE', #2272, .T. ) ;
#5307 = AXIS2_PLACEMENT_3D ( 'NONE', #9549, #6578, #5798 ) ;
#5308 = CARTESIAN_POINT ( 'NONE',  ( 1.138917931912835794E-26, 58.00000000000029132, -25.00000000000000000 ) ) ;
#5309 = CIRCLE ( 'NONE', #5918, 25.00000000000000000 ) ;
#5310 = ORIENTED_EDGE ( 'NONE', *, *, #4331, .F. ) ;
#5311 = DIRECTION ( 'NONE',  ( -0.000000000000000000, 1.000000000000000000, 0.000000000000000000 ) ) ;
#5312 = ORIENTED_EDGE ( 'NONE', *, *, #1533, .F. ) ;
#5313 = ORIENTED_EDGE ( 'NONE', *, *, #9581, .F. ) ;
#5314 = CARTESIAN_POINT ( 'NONE',  ( 0.000000000000000000, 54.99999999999999289, -33.00000000000000711 ) ) ;
#5315 = CARTESIAN_POINT ( 'NONE',  ( -0.9115637956585259660, -11.70315718320097886, 38.99939858132674431 ) ) ;
#5316 = CARTESIAN_POINT ( 'NONE',  ( 26.33333333333338544, 26.33333333333327886, 1.333333333333379001 ) ) ;
#5317 = VECTOR ( 'NONE', #7948, 1000.000000000000000 ) ;
#5318 = CARTESIAN_POINT ( 'NONE',  ( 0.000000000000000000, 61.99999999999999289, 0.000000000000000000 ) ) ;
#5319 = EDGE_CURVE ( 'NONE', #1356, #4632, #8840, .T. ) ;
#5320 = EDGE_LOOP ( 'NONE', ( #1634, #9295, #7744, #4775, #5680, #9338, #6745, #7797, #5428, #4370, #5139 ) ) ;
#5321 = CARTESIAN_POINT ( 'NONE',  ( 0.000000000000000000, 30.00000000000000000, 0.000000000000000000 ) ) ;
#5322 = VERTEX_POINT ( 'NONE', #4330 ) ;
#5323 = CARTESIAN_POINT ( 'NONE',  ( -8.216777476527294510, 44.50000000000019185, -23.61111111111111427 ) ) ;
#5324 = DIRECTION ( 'NONE',  ( 0.000000000000000000, 0.000000000000000000, 1.000000000000000000 ) ) ;
#5325 = FACE_OUTER_BOUND ( 'NONE', #4174, .T. ) ;
#5326 = LINE ( 'NONE', #3638, #2618 ) ;
#5327 = CARTESIAN_POINT ( 'NONE',  ( 12.20000000000000107, 0.000000000000000000, 1.610000000000000098 ) ) ;
#5328 = ORIENTED_EDGE ( 'NONE', *, *, #6175, .T. ) ;
#5329 = LINE ( 'NONE', #3843, #5122 ) ;
#5330 = FACE_OUTER_BOUND ( 'NONE', #9136, .T. ) ;
#5331 = ORIENTED_EDGE ( 'NONE', *, *, #2685, .F. ) ;
#5332 = CARTESIAN_POINT ( 'NONE',  ( -10.00000000000001599, 3.294852476658805873, 41.36423575989289247 ) ) ;
#5333 = ORIENTED_EDGE ( 'NONE', *, *, #9565, .T. ) ;
#5334 = DIRECTION ( 'NONE',  ( 0.000000000000000000, 0.000000000000000000, 1.000000000000000000 ) ) ;
#5335 = CARTESIAN_POINT ( 'NONE',  ( 5.824897344823916079, -8.145636269817515540, 38.91941837930603754 ) ) ;
#5336 = EDGE_LOOP ( 'NONE', ( #4571, #2524, #8701, #4109, #700, #3217 ) ) ;
#5337 = EDGE_CURVE ( 'NONE', #5461, #928, #4284, .T. ) ;
#5338 = CARTESIAN_POINT ( 'NONE',  ( -8.216777476527274970, 78.08723716182652197, -23.61111111111111427 ) ) ;
#5339 = CARTESIAN_POINT ( 'NONE',  ( 0.000000000000000000, 3.294852476641296768, 184.6745183374407020 ) ) ;
#5340 = ORIENTED_EDGE ( 'NONE', *, *, #3525, .T. ) ;
#5341 = CARTESIAN_POINT ( 'NONE',  ( 9.998295632719816695, 2.529332002499826704, 37.85922636131657271 ) ) ;
#5342 = ORIENTED_EDGE ( 'NONE', *, *, #4278, .T. ) ;
#5343 = LINE ( 'NONE', #3809, #1038 ) ;
#5344 = EDGE_CURVE ( 'NONE', #903, #5641, #6538, .T. ) ;
#5345 = DIRECTION ( 'NONE',  ( 0.07726494571055114724, 0.000000000000000000, 0.9970105958134776181 ) ) ;
#5346 = CARTESIAN_POINT ( 'NONE',  ( 25.51470164434615029, 30.00000000000000000, 5.000000000000000888 ) ) ;
#5347 = ORIENTED_EDGE ( 'NONE', *, *, #5226, .F. ) ;
#5348 = PLANE ( 'NONE',  #8615 ) ;
#5349 = ORIENTED_EDGE ( 'NONE', *, *, #9609, .T. ) ;
#5350 = EDGE_CURVE ( 'NONE', #4048, #7113, #4119, .T. ) ;
#5351 = FACE_OUTER_BOUND ( 'NONE', #6804, .T. ) ;
#5352 = LINE ( 'NONE', #8409, #8294 ) ;
#5353 = CARTESIAN_POINT ( 'NONE',  ( -24.67792535850613334, 28.99999999999997158, 4.000000000000009770 ) ) ;
#5354 = EDGE_CURVE ( 'NONE', #5049, #6362, #2786, .T. ) ;
#5355 = ADVANCED_FACE ( 'NONE', ( #1403 ), #2831, .T. ) ;
#5356 = ORIENTED_EDGE ( 'NONE', *, *, #8610, .T. ) ;
#5357 = CARTESIAN_POINT ( 'NONE',  ( -8.545448575588403983, 42.50000000000020606, -24.55555555555568858 ) ) ;
#5358 = EDGE_CURVE ( 'NONE', #4065, #8074, #6938, .T. ) ;
#5359 = EDGE_LOOP ( 'NONE', ( #3715, #3814, #3748, #6623 ) ) ;
#5360 = ORIENTED_EDGE ( 'NONE', *, *, #5826, .T. ) ;
#5361 = PLANE ( 'NONE',  #1648 ) ;
#5362 = CARTESIAN_POINT ( 'NONE',  ( 0.000000000000000000, 3.294852476641296768, 294.6136752714472777 ) ) ;
#5363 = CARTESIAN_POINT ( 'NONE',  ( -28.87459861216645862, 61.99999999999999289, -14.47678174684361352 ) ) ;
#5364 = AXIS2_PLACEMENT_3D ( 'NONE', #488, #2045, #6399 ) ;
#5365 = CIRCLE ( 'NONE', #2347, 4.999999999999997335 ) ;
#5366 = VECTOR ( 'NONE', #422, 1000.000000000000000 ) ;
#5367 = ORIENTED_EDGE ( 'NONE', *, *, #538, .F. ) ;
#5368 = FACE_OUTER_BOUND ( 'NONE', #9649, .T. ) ;
#5369 = CARTESIAN_POINT ( 'NONE',  ( 0.000000000000000000, 39.99999999999999289, 0.000000000000000000 ) ) ;
#5370 = CARTESIAN_POINT ( 'NONE',  ( -5.562309845551829390, 59.00253480853272947, 35.56426808735054834 ) ) ;
#5371 = ORIENTED_EDGE ( 'NONE', *, *, #6106, .T. ) ;
#5372 = CARTESIAN_POINT ( 'NONE',  ( 1.314778108344340835, -6.640250172933917838, 43.96652902435248933 ) ) ;
#5373 = CARTESIAN_POINT ( 'NONE',  ( 8.063708916478045552, 59.93271281907998826, -32.87005020308307479 ) ) ;
#5374 = DIRECTION ( 'NONE',  ( 0.000000000000000000, 0.000000000000000000, 1.000000000000000000 ) ) ;
#5375 = CARTESIAN_POINT ( 'NONE',  ( 1.555535097482682654E-26, 78.08723716182652197, -25.00000000000000000 ) ) ;
#5376 = DIRECTION ( 'NONE',  ( 0.000000000000000000, 0.8660254037844385966, 0.5000000000000003331 ) ) ;
#5377 = ORIENTED_EDGE ( 'NONE', *, *, #8614, .T. ) ;
#5378 = AXIS2_PLACEMENT_3D ( 'NONE', #6974, #1704, #4581 ) ;
#5379 = CARTESIAN_POINT ( 'NONE',  ( 18.58791755254457811, 59.99999999999999289, 23.54759692749571443 ) ) ;
#5380 = VECTOR ( 'NONE', #8078, 1000.000000000000114 ) ;
#5381 = ORIENTED_EDGE ( 'NONE', *, *, #9033, .F. ) ;
#5382 = CARTESIAN_POINT ( 'NONE',  ( 1.040310318760209318E-26, 50.00000000000032685, -26.00000000000009592 ) ) ;
#5383 = ORIENTED_EDGE ( 'NONE', *, *, #4387, .F. ) ;
#5384 = DIRECTION ( 'NONE',  ( 0.7849198975831889191, -0.000000000000000000, -0.6195972517514874989 ) ) ;
#5385 = CARTESIAN_POINT ( 'NONE',  ( 1.066084653997754650, -14.99999999999968203, 36.76550911089076124 ) ) ;
#5386 = ORIENTED_EDGE ( 'NONE', *, *, #235, .F. ) ;
#5387 = AXIS2_PLACEMENT_3D ( 'NONE', #6394, #2040, #5754 ) ;
#5388 = LINE ( 'NONE', #4603, #5081 ) ;
#5389 = CARTESIAN_POINT ( 'NONE',  ( -6.000000000000005329, 29.14236109046821710, -29.24912810952613640 ) ) ;
#5390 = ORIENTED_EDGE ( 'NONE', *, *, #6063, .F. ) ;
#5391 = CARTESIAN_POINT ( 'NONE',  ( 9.872059229381315859, 4.922636072021620457, 41.43345053423059454 ) ) ;
#5392 = AXIS2_PLACEMENT_3D ( 'NONE', #5044, #1202, #5789 ) ;
#5393 = EDGE_CURVE ( 'NONE', #2908, #1478, #1429, .T. ) ;
#5394 = EDGE_LOOP ( 'NONE', ( #4033, #9291, #3908, #3129 ) ) ;
#5395 = DIRECTION ( 'NONE',  ( 0.000000000000000000, 1.000000000000000000, 0.000000000000000000 ) ) ;
#5396 = DIRECTION ( 'NONE',  ( -1.000000000000000000, 0.000000000000000000, 0.000000000000000000 ) ) ;
#5397 = VERTEX_POINT ( 'NONE', #3627 ) ;
#5398 = CYLINDRICAL_SURFACE ( 'NONE', #7510, 31.49999999999999289 ) ;
#5399 = VECTOR ( 'NONE', #2051, 1000.000000000000000 ) ;
#5400 = ORIENTED_EDGE ( 'NONE', *, *, #1606, .T. ) ;
#5401 = CARTESIAN_POINT ( 'NONE',  ( -29.82695610816121956, 59.99999999999999289, 23.54469556655648432 ) ) ;
#5402 = CARTESIAN_POINT ( 'NONE',  ( 24.96033808169876878, 29.33187429063046991, -4.331874290630493896 ) ) ;
#5403 = DIRECTION ( 'NONE',  ( -0.000000000000000000, 1.000000000000000000, -0.000000000000000000 ) ) ;
#5404 = VECTOR ( 'NONE', #1146, 1000.000000000000000 ) ;
#5405 = ORIENTED_EDGE ( 'NONE', *, *, #9018, .F. ) ;
#5406 = ORIENTED_EDGE ( 'NONE', *, *, #7972, .F. ) ;
#5407 = DIRECTION ( 'NONE',  ( 1.735493991486225972E-29, -6.508102468073347395E-30, -1.000000000000000000 ) ) ;
#5408 = ORIENTED_EDGE ( 'NONE', *, *, #5936, .T. ) ;
#5409 = ORIENTED_EDGE ( 'NONE', *, *, #5166, .T. ) ;
#5410 = DIRECTION ( 'NONE',  ( 1.735493991486225972E-29, -6.508102468073347395E-30, -1.000000000000000000 ) ) ;
#5411 = CIRCLE ( 'NONE', #211, 40.00000000000000711 ) ;
#5412 = ADVANCED_FACE ( 'NONE', ( #2881 ), #6465, .T. ) ;
#5413 = EDGE_CURVE ( 'NONE', #1128, #2408, #183, .T. ) ;
#5414 =( NAMED_UNIT ( * ) PLANE_ANGLE_UNIT ( ) SI_UNIT ( $, .RADIAN. ) );
#5415 = ADVANCED_FACE ( 'NONE', ( #8270 ), #9013, .F. ) ;
#5416 = ADVANCED_FACE ( 'NONE', ( #768 ), #5361, .F. ) ;
#5417 = PLANE ( 'NONE',  #8081 ) ;
#5418 = CIRCLE ( 'NONE', #3517, 1.899999999999999689 ) ;
#5419 = VERTEX_POINT ( 'NONE', #232 ) ;
#5420 = PLANE ( 'NONE',  #8988 ) ;
#5421 = DIRECTION ( 'NONE',  ( 0.000000000000000000, 0.000000000000000000, 1.000000000000000000 ) ) ;
#5422 = VECTOR ( 'NONE', #3043, 1000.000000000000000 ) ;
#5423 = ORIENTED_EDGE ( 'NONE', *, *, #6106, .F. ) ;
#5424 = CARTESIAN_POINT ( 'NONE',  ( 2.604746439356475207, -6.365628610964990663, 43.82878309350103763 ) ) ;
#5425 = DIRECTION ( 'NONE',  ( 0.000000000000000000, 0.000000000000000000, 1.000000000000000000 ) ) ;
#5426 = LINE ( 'NONE', #7078, #2381 ) ;
#5427 = DIRECTION ( 'NONE',  ( 0.000000000000000000, 0.000000000000000000, 1.000000000000000000 ) ) ;
#5428 = ORIENTED_EDGE ( 'NONE', *, *, #2796, .F. ) ;
#5429 = CARTESIAN_POINT ( 'NONE',  ( -31.00000000000001066, 27.61361909880193011, 5.005767756411737324 ) ) ;
#5430 = DIRECTION ( 'NONE',  ( -1.820952055660014662E-28, -1.000000000000000000, -7.038118388768679669E-30 ) ) ;
#5431 = ORIENTED_EDGE ( 'NONE', *, *, #9215, .F. ) ;
#5432 = CARTESIAN_POINT ( 'NONE',  ( 1.148778693228098442E-26, 57.50000000000029843, -25.00000000000000000 ) ) ;
#5433 = LINE ( 'NONE', #2597, #6400 ) ;
#5434 = ORIENTED_EDGE ( 'NONE', *, *, #761, .T. ) ;
#5435 = VECTOR ( 'NONE', #9270, 1000.000000000000000 ) ;
#5436 = DIRECTION ( 'NONE',  ( -0.000000000000000000, 1.000000000000000000, -0.000000000000000000 ) ) ;
#5437 = VECTOR ( 'NONE', #7346, 1000.000000000000000 ) ;
#5438 =( REPRESENTATION_RELATIONSHIP ('NONE','NONE', #5841, #1483 ) REPRESENTATION_RELATIONSHIP_WITH_TRANSFORMATION ( #3201 )SHAPE_REPRESENTATION_RELATIONSHIP( ) );
#5439 = LINE ( 'NONE', #8448, #5134 ) ;
#5440 = ORIENTED_EDGE ( 'NONE', *, *, #3530, .F. ) ;
#5441 = CARTESIAN_POINT ( 'NONE',  ( 4.433825966365425586, -5.692418513649885270, 43.50410792870121668 ) ) ;
#5442 = ADVANCED_FACE ( 'NONE', ( #3882 ), #3021, .F. ) ;
#5443 = CARTESIAN_POINT ( 'NONE',  ( -28.34870838944214100, 39.99999999999999289, -9.815840903884556212 ) ) ;
#5444 = VECTOR ( 'NONE', #7247, 1000.000000000000000 ) ;
#5445 = DIRECTION ( 'NONE',  ( 0.9444444444444443088, -0.000000000000000000, -0.3286710990610907657 ) ) ;
#5446 = FACE_OUTER_BOUND ( 'NONE', #8318, .T. ) ;
#5447 = ORIENTED_EDGE ( 'NONE', *, *, #93, .F. ) ;
#5448 = LINE ( 'NONE', #6954, #900 ) ;
#5449 = VECTOR ( 'NONE', #6411, 1000.000000000000000 ) ;
#5450 = EDGE_LOOP ( 'NONE', ( #5034, #8551, #8438, #3999 ) ) ;
#5451 = DIRECTION ( 'NONE',  ( -0.000000000000000000, 1.000000000000000000, -0.000000000000000000 ) ) ;
#5452 = CARTESIAN_POINT ( 'NONE',  ( -5.562309845534701758, 61.83753588906734677, 37.56426808735052703 ) ) ;
#5453 = AXIS2_PLACEMENT_3D ( 'NONE', #6215, #9249, #1330 ) ;
#5454 = AXIS2_PLACEMENT_3D ( 'NONE', #1949, #6290, #4925 ) ;
#5455 = ORIENTED_EDGE ( 'NONE', *, *, #8532, .T. ) ;
#5456 = FACE_OUTER_BOUND ( 'NONE', #841, .T. ) ;
#5457 = VECTOR ( 'NONE', #8702, 1000.000000000000000 ) ;
#5458 = ORIENTED_EDGE ( 'NONE', *, *, #3540, .T. ) ;
#5459 = AXIS2_PLACEMENT_3D ( 'NONE', #2070, #5876, #6518 ) ;
#5460 = VECTOR ( 'NONE', #8139, 1000.000000000000000 ) ;
#5461 = VERTEX_POINT ( 'NONE', #8472 ) ;
#5462 = CIRCLE ( 'NONE', #816, 3.799999999999999378 ) ;
#5463 = CARTESIAN_POINT ( 'NONE',  ( -5.042085649091919919, -5.365591822504794273, 43.35300965850710497 ) ) ;
#5464 = FACE_OUTER_BOUND ( 'NONE', #2111, .T. ) ;
#5465 = ADVANCED_FACE ( 'NONE', ( #3172 ), #2332, .F. ) ;
#5466 = CARTESIAN_POINT ( 'NONE',  ( 18.58791755254457811, 39.99999999999999289, 23.54759692749571443 ) ) ;
#5467 = VECTOR ( 'NONE', #6834, 999.9999999999998863 ) ;
#5468 = ORIENTED_EDGE ( 'NONE', *, *, #5995, .F. ) ;
#5469 = CARTESIAN_POINT ( 'NONE',  ( 0.000000000000000000, -50.91168824543140659, 0.000000000000000000 ) ) ;
#5470 = LINE ( 'NONE', #6928, #171 ) ;
#5471 = ADVANCED_FACE ( 'NONE', ( #138 ), #2379, .T. ) ;
#5472 = EDGE_LOOP ( 'NONE', ( #7678, #6189, #7255, #4070 ) ) ;
#5473 = EDGE_CURVE ( 'NONE', #8960, #1381, #3383, .T. ) ;
#5474 = CARTESIAN_POINT ( 'NONE',  ( 3.106744199778904925, 59.95265069314689299, -33.56539760714087350 ) ) ;
#5475 = CIRCLE ( 'NONE', #9104, 25.00000000000000000 ) ;
#5476 = FACE_OUTER_BOUND ( 'NONE', #494, .T. ) ;
#5477 = FACE_OUTER_BOUND ( 'NONE', #8377, .T. ) ;
#5478 = EDGE_CURVE ( 'NONE', #8947, #5781, #9066, .T. ) ;
#5479 = PLANE ( 'NONE',  #2992 ) ;
#5480 = ORIENTED_EDGE ( 'NONE', *, *, #4319, .T. ) ;
#5481 = LINE ( 'NONE', #8387, #7806 ) ;
#5482 = ADVANCED_FACE ( 'NONE', ( #6771 ), #6899, .F. ) ;
#5483 = VECTOR ( 'NONE', #3634, 1000.000000000000000 ) ;
#5484 = PLANE ( 'NONE',  #1642 ) ;
#5485 = EDGE_CURVE ( 'NONE', #2731, #5636, #9547, .T. ) ;
#5486 = ORIENTED_EDGE ( 'NONE', *, *, #3461, .T. ) ;
#5487 = DIRECTION ( 'NONE',  ( 0.000000000000000000, -1.000000000000000000, 0.000000000000000000 ) ) ;
#5488 = CARTESIAN_POINT ( 'NONE',  ( 28.34870838944214100, 59.99999999999999289, 9.815840903884559765 ) ) ;
#5489 = ORIENTED_EDGE ( 'NONE', *, *, #5619, .T. ) ;
#5490 = EDGE_CURVE ( 'NONE', #5397, #3415, #5248, .T. ) ;
#5491 = CARTESIAN_POINT ( 'NONE',  ( 0.000000000000000000, -15.00000000000000000, 0.000000000000000000 ) ) ;
#5492 = DIRECTION ( 'NONE',  ( 0.000000000000000000, 1.000000000000000000, 0.000000000000000000 ) ) ;
#5493 = ORIENTED_EDGE ( 'NONE', *, *, #4154, .T. ) ;
#5494 = CARTESIAN_POINT ( 'NONE',  ( -31.00000000000000711, -15.00000000000000000, -5.999999999999996447 ) ) ;
#5495 = CYLINDRICAL_SURFACE ( 'NONE', #7191, 38.00000000000000711 ) ;
#5496 = ORIENTED_EDGE ( 'NONE', *, *, #3441, .T. ) ;
#5497 = CARTESIAN_POINT ( 'NONE',  ( 8.237197373723128990, -4.999999999999999112, 27.80554943579302574 ) ) ;
#5498 = CARTESIAN_POINT ( 'NONE',  ( -5.999999999999998224, -15.00000000000000000, 26.32489316217636954 ) ) ;
#5499 = B_SPLINE_CURVE_WITH_KNOTS ( 'NONE', 3,
 ( #2146, #8084, #1226, #3487, #9518, #2002 ),
 .UNSPECIFIED., .F., .F.,
 ( 4, 2, 4 ),
 ( 0.000000000000000000, 0.0005212762617847652939, 0.001042552523569530588 ),
 .UNSPECIFIED. ) ;
#5500 = ORIENTED_EDGE ( 'NONE', *, *, #5358, .F. ) ;
#5501 = DIRECTION ( 'NONE',  ( 1.000000000000000000, 0.000000000000000000, -1.084202172485503448E-16 ) ) ;
#5502 = EDGE_CURVE ( 'NONE', #6350, #7928, #8339, .T. ) ;
#5503 = CARTESIAN_POINT ( 'NONE',  ( -2.637864787425444835, -6.356637827719301193, 43.82432124711748855 ) ) ;
#5504 = ORIENTED_EDGE ( 'NONE', *, *, #163, .T. ) ;
#5505 = CARTESIAN_POINT ( 'NONE',  ( -34.30759795839968262, 59.50675430643739361, -7.737048950318285101 ) ) ;
#5506 = VERTEX_POINT ( 'NONE', #7619 ) ;
#5507 = DIRECTION ( 'NONE',  ( 0.000000000000000000, -1.000000000000000000, 0.000000000000000000 ) ) ;
#5508 = ORIENTED_EDGE ( 'NONE', *, *, #8130, .F. ) ;
#5509 = CARTESIAN_POINT ( 'NONE',  ( -6.323936101127149989, -4.493502404820619134, 38.59188261056448965 ) ) ;
#5510 = DIRECTION ( 'NONE',  ( -0.1666666666666658525, -3.897465909857536228E-29, -0.9860132971832695770 ) ) ;
#5511 = CYLINDRICAL_SURFACE ( 'NONE', #6023, 2.500000000000002220 ) ;
#5512 = EDGE_LOOP ( 'NONE', ( #1733, #9737, #5092, #866, #5298 ) ) ;
#5513 = CYLINDRICAL_SURFACE ( 'NONE', #6764, 3.799999999999999378 ) ;
#5514 = ADVANCED_FACE ( 'NONE', ( #5351 ), #3815, .F. ) ;
#5515 = CARTESIAN_POINT ( 'NONE',  ( 4.776122516674680244E-15, 19.99999999999982236, 39.00000000000002132 ) ) ;
#5516 = CARTESIAN_POINT ( 'NONE',  ( 3.850561375233632511, 59.53730689706333834, -34.89414954626303000 ) ) ;
#5517 = FACE_OUTER_BOUND ( 'NONE', #5022, .T. ) ;
#5518 = CARTESIAN_POINT ( 'NONE',  ( -8.216777476527294510, 58.00000000000029132, -23.61111111111107519 ) ) ;
#5519 = LINE ( 'NONE', #7643, #7800 ) ;
#5520 = CIRCLE ( 'NONE', #4418, 31.49999999999999289 ) ;
#5521 = VECTOR ( 'NONE', #4423, 1000.000000000000114 ) ;
#5522 = EDGE_CURVE ( 'NONE', #6324, #2298, #4336, .T. ) ;
#5523 = CIRCLE ( 'NONE', #8196, 39.00000000000002132 ) ;
#5524 = LINE ( 'NONE', #4879, #862 ) ;
#5525 = EDGE_LOOP ( 'NONE', ( #6295, #3973 ) ) ;
#5526 = DIRECTION ( 'NONE',  ( 0.000000000000000000, 0.000000000000000000, 1.000000000000000000 ) ) ;
#5527 = CARTESIAN_POINT ( 'NONE',  ( 35.86802812777743554, 61.99999999999999289, 9.082100980773358145 ) ) ;
#5528 = ORIENTED_EDGE ( 'NONE', *, *, #8060, .F. ) ;
#5529 = EDGE_CURVE ( 'NONE', #2376, #2208, #6866, .T. ) ;
#5530 = DIRECTION ( 'NONE',  ( -0.000000000000000000, 1.000000000000000000, -0.000000000000000000 ) ) ;
#5531 = ADVANCED_FACE ( 'NONE', ( #5303 ), #9695, .T. ) ;
#5532 = AXIS2_PLACEMENT_3D ( 'NONE', #444, #9425, #7935 ) ;
#5533 = EDGE_CURVE ( 'NONE', #8554, #3288, #3113, .T. ) ;
#5534 = CARTESIAN_POINT ( 'NONE',  ( -37.42097066196858179, 61.92370482830305889, -4.403127714044224206 ) ) ;
#5535 = CARTESIAN_POINT ( 'NONE',  ( 8.758195361064911921, -8.001464458227651733, 38.00543791605778665 ) ) ;
#5536 = CARTESIAN_POINT ( 'NONE',  ( -12.43339847825378719, 54.99999999999999289, 35.90836395996003461 ) ) ;
#5537 = PRESENTATION_LAYER_ASSIGNMENT (  '', '', ( #1599 ) ) ;
#5538 = ORIENTED_EDGE ( 'NONE', *, *, #9095, .F. ) ;
#5539 = DIRECTION ( 'NONE',  ( 0.000000000000000000, 0.000000000000000000, 1.000000000000000000 ) ) ;
#5540 = ORIENTED_EDGE ( 'NONE', *, *, #3736, .F. ) ;
#5541 = CARTESIAN_POINT ( 'NONE',  ( 35.88888888888889284, 54.99999999999999289, -12.48950176432140502 ) ) ;
#5542 = ORIENTED_EDGE ( 'NONE', *, *, #8666, .F. ) ;
#5543 = DIRECTION ( 'NONE',  ( -1.000000000000000000, 0.000000000000000000, 0.000000000000000000 ) ) ;
#5544 = DIRECTION ( 'NONE',  ( -0.7849198975831893632, -0.000000000000000000, 0.6195972517514870548 ) ) ;
#5545 = AXIS2_PLACEMENT_3D ( 'NONE', #6194, #3276, #2579 ) ;
#5546 = LINE ( 'NONE', #7058, #7085 ) ;
#5547 = ORIENTED_EDGE ( 'NONE', *, *, #2925, .T. ) ;
#5548 = DIRECTION ( 'NONE',  ( 0.000000000000000000, 0.000000000000000000, 1.000000000000000000 ) ) ;
#5549 = EDGE_LOOP ( 'NONE', ( #2304, #4868, #593, #9699 ) ) ;
#5550 = DIRECTION ( 'NONE',  ( 0.000000000000000000, 1.000000000000000000, 0.000000000000000000 ) ) ;
#5551 = ORIENTED_EDGE ( 'NONE', *, *, #2180, .F. ) ;
#5552 = CARTESIAN_POINT ( 'NONE',  ( -12.59566441936335757, -1.532720036839458899, 36.91025998118985996 ) ) ;
#5553 = CARTESIAN_POINT ( 'NONE',  ( 0.000000000000000000, 30.00000000000000000, 0.000000000000000000 ) ) ;
#5554 = VECTOR ( 'NONE', #2708, 1000.000000000000000 ) ;
#5555 = CARTESIAN_POINT ( 'NONE',  ( 1.099474886651785204E-26, 56.50000000000029843, -37.00000000000000711 ) ) ;
#5556 = ORIENTED_EDGE ( 'NONE', *, *, #6366, .F. ) ;
#5557 = DIRECTION ( 'NONE',  ( -0.000000000000000000, -1.000000000000000000, -0.000000000000000000 ) ) ;
#5558 = EDGE_LOOP ( 'NONE', ( #7451, #1099, #8769, #3445 ) ) ;
#5559 = DIRECTION ( 'NONE',  ( 0.000000000000000000, 1.000000000000000000, 0.000000000000000000 ) ) ;
#5560 = AXIS2_PLACEMENT_3D ( 'NONE', #6852, #2999, #7 ) ;
#5561 = CARTESIAN_POINT ( 'NONE',  ( 1.820000000000000062, 0.000000000000000000, 3.799999999999999378 ) ) ;
#5562 = CARTESIAN_POINT ( 'NONE',  ( -997.9783121635130101, 0.000000000000000000, 0.000000000000000000 ) ) ;
#5563 =( NAMED_UNIT ( * ) PLANE_ANGLE_UNIT ( ) SI_UNIT ( $, .RADIAN. ) );
#5564 = CARTESIAN_POINT ( 'NONE',  ( 15.25056439471407188, 60.99999999999999289, -27.56211685706813341 ) ) ;
#5565 = LINE ( 'NONE', #1170, #2115 ) ;
#5566 = VECTOR ( 'NONE', #75, 1000.000000000000000 ) ;
#5567 = VECTOR ( 'NONE', #6203, 1000.000000000000000 ) ;
#5568 = LINE ( 'NONE', #9367, #3623 ) ;
#5569 = ORIENTED_EDGE ( 'NONE', *, *, #8502, .T. ) ;
#5570 = CARTESIAN_POINT ( 'NONE',  ( 1.028855784077797189E-26, 56.50000000000029843, 3.062228611575705006E-28 ) ) ;
#5571 = ORIENTED_EDGE ( 'NONE', *, *, #8234, .T. ) ;
#5572 = DIRECTION ( 'NONE',  ( 0.000000000000000000, 1.000000000000000000, 0.000000000000000000 ) ) ;
#5573 = CARTESIAN_POINT ( 'NONE',  ( -5.000000000000006217, 30.00000000000000000, -25.51470164434615029 ) ) ;
#5574 = ORIENTED_EDGE ( 'NONE', *, *, #1061, .T. ) ;
#5575 = CARTESIAN_POINT ( 'NONE',  ( -15.97678174684350871, 60.99999999999999289, 28.87459861216650836 ) ) ;
#5576 = CARTESIAN_POINT ( 'NONE',  ( 8.673617379884035472E-16, 30.00000000000000000, 4.000000000000004441 ) ) ;
#5577 = DIRECTION ( 'NONE',  ( 0.000000000000000000, 0.000000000000000000, 1.000000000000000000 ) ) ;
#5578 = LINE ( 'NONE', #6211, #8516 ) ;
#5579 = DIRECTION ( 'NONE',  ( 0.000000000000000000, 0.000000000000000000, 1.000000000000000000 ) ) ;
#5580 = ADVANCED_FACE ( 'NONE', ( #3764 ), #4793, .F. ) ;
#5581 = EDGE_CURVE ( 'NONE', #3464, #427, #9327, .T. ) ;
#5582 = ORIENTED_EDGE ( 'NONE', *, *, #586, .T. ) ;
#5583 = CARTESIAN_POINT ( 'NONE',  ( -8.545448575588384443, 52.00000000000031974, -24.55555555555561753 ) ) ;
#5584 = LINE ( 'NONE', #6268, #3091 ) ;
#5585 = EDGE_CURVE ( 'NONE', #5689, #9409, #6757, .T. ) ;
#5586 = ORIENTED_EDGE ( 'NONE', *, *, #6720, .F. ) ;
#5587 = AXIS2_PLACEMENT_3D ( 'NONE', #8982, #5276, #2151 ) ;
#5588 = CARTESIAN_POINT ( 'NONE',  ( -4.999999999999999112, 30.00000000000000000, 30.00000000000000711 ) ) ;
#5589 = DIRECTION ( 'NONE',  ( 1.735493991486225972E-29, -6.508102468073347395E-30, -1.000000000000000000 ) ) ;
#5590 = VECTOR ( 'NONE', #9055, 1000.000000000000114 ) ;
#5591 = CIRCLE ( 'NONE', #2584, 4.500000000000005329 ) ;
#5592 = VERTEX_POINT ( 'NONE', #18 ) ;
#5593 = CARTESIAN_POINT ( 'NONE',  ( 9.318419442923201951E-27, 49.00000000000032685, -26.00000000000009592 ) ) ;
#5594 = ADVANCED_FACE ( 'NONE', ( #8643 ), #3860, .T. ) ;
#5595 = ORIENTED_EDGE ( 'NONE', *, *, #6490, .T. ) ;
#5596 = FACE_OUTER_BOUND ( 'NONE', #9532, .T. ) ;
#5597 = ORIENTED_EDGE ( 'NONE', *, *, #4438, .F. ) ;
#5598 = VERTEX_POINT ( 'NONE', #6500 ) ;
#5599 = ADVANCED_FACE ( 'NONE', ( #1279 ), #2750, .T. ) ;
#5600 = CARTESIAN_POINT ( 'NONE',  ( -8.684397385907152156, -1.706296020601628216, 42.03131819750302611 ) ) ;
#5601 = VECTOR ( 'NONE', #6953, 1000.000000000000114 ) ;
#5602 = DIRECTION ( 'NONE',  ( 0.000000000000000000, 0.000000000000000000, 1.000000000000000000 ) ) ;
#5603 = VECTOR ( 'NONE', #6588, 1000.000000000000000 ) ;
#5604 = PLANE ( 'NONE',  #6817 ) ;
#5605 = AXIS2_PLACEMENT_3D ( 'NONE', #2357, #9098, #1631 ) ;
#5606 = CIRCLE ( 'NONE', #8132, 26.00000000000000355 ) ;
#5607 = ORIENTED_EDGE ( 'NONE', *, *, #1184, .F. ) ;
#5608 = CARTESIAN_POINT ( 'NONE',  ( 9.762153702110021092E-27, 48.50000000000033396, -24.09806918451532809 ) ) ;
#5609 = AXIS2_PLACEMENT_3D ( 'NONE', #3084, #3740, #5324 ) ;
#5610 = AXIS2_PLACEMENT_3D ( 'NONE', #1794, #3324, #3431 ) ;
#5611 = ORIENTED_EDGE ( 'NONE', *, *, #6224, .T. ) ;
#5612 = CARTESIAN_POINT ( 'NONE',  ( 0.000000000000000000, 0.000000000000000000, 0.000000000000000000 ) ) ;
#5613 = DIRECTION ( 'NONE',  ( 1.735493991486225972E-29, -6.508102468073347395E-30, -1.000000000000000000 ) ) ;
#5614 = LINE ( 'NONE', #2483, #8981 ) ;
#5615 = CARTESIAN_POINT ( 'NONE',  ( 11.24085533630444544, -4.722505971463051289, 37.34530973190163650 ) ) ;
#5616 = FACE_OUTER_BOUND ( 'NONE', #4907, .T. ) ;
#5617 = LINE ( 'NONE', #1858, #5753 ) ;
#5618 = AXIS2_PLACEMENT_3D ( 'NONE', #1687, #1042, #3202 ) ;
#5619 = EDGE_CURVE ( 'NONE', #8688, #3761, #8746, .T. ) ;
#5620 = AXIS2_PLACEMENT_3D ( 'NONE', #5246, #1735, #6168 ) ;
#5621 = ORIENTED_EDGE ( 'NONE', *, *, #1421, .F. ) ;
#5622 = FACE_OUTER_BOUND ( 'NONE', #1578, .T. ) ;
#5623 = CARTESIAN_POINT ( 'NONE',  ( -997.9783121635130101, 0.000000000000000000, 0.000000000000000000 ) ) ;
#5624 = B_SPLINE_CURVE_WITH_KNOTS ( 'NONE', 3,
 ( #2988, #2186, #5954, #5997 ),
 .UNSPECIFIED., .F., .F.,
 ( 4, 4 ),
 ( 8.673617379884035472E-19, 0.006018989108141225772 ),
 .UNSPECIFIED. ) ;
#5625 = ORIENTED_EDGE ( 'NONE', *, *, #1544, .T. ) ;
#5626 = DIRECTION ( 'NONE',  ( 0.000000000000000000, 0.000000000000000000, 1.000000000000000000 ) ) ;
#5627 = DIRECTION ( 'NONE',  ( -0.000000000000000000, -1.000000000000000000, -0.000000000000000000 ) ) ;
#5628 = EDGE_LOOP ( 'NONE', ( #6583, #4006, #3768, #3176 ) ) ;
#5629 = DIRECTION ( 'NONE',  ( -0.000000000000000000, 1.000000000000000000, -0.000000000000000000 ) ) ;
#5630 = DIRECTION ( 'NONE',  ( 0.000000000000000000, 1.000000000000000000, 0.000000000000000000 ) ) ;
#5631 = AXIS2_PLACEMENT_3D ( 'NONE', #3087, #7397, #4589 ) ;
#5632 = LINE ( 'NONE', #7861, #9252 ) ;
#5633 = CARTESIAN_POINT ( 'NONE',  ( 8.083702140090636590, -8.624291467721789672, 38.15459417795183583 ) ) ;
#5634 = ORIENTED_EDGE ( 'NONE', *, *, #5502, .T. ) ;
#5635 = CARTESIAN_POINT ( 'NONE',  ( 1.300000000000000044, 3.252606517456513302E-16, 2.499999999999999556 ) ) ;
#5636 = VERTEX_POINT ( 'NONE', #1082 ) ;
#5637 = LINE ( 'NONE', #8649, #2271 ) ;
#5638 = VERTEX_POINT ( 'NONE', #6450 ) ;
#5639 = CARTESIAN_POINT ( 'NONE',  ( 32.05305536707737701, 59.99999999999999289, 7.848671329280705322 ) ) ;
#5640 = ADVANCED_FACE ( 'NONE', ( #5772 ), #395, .F. ) ;
#5641 = VERTEX_POINT ( 'NONE', #9478 ) ;
#5642 = CARTESIAN_POINT ( 'NONE',  ( 20.99999999999999645, 0.000000000000000000, -4.000000000000006217 ) ) ;
#5643 = DIRECTION ( 'NONE',  ( 1.000000000000000000, 0.000000000000000000, 1.079383496163345602E-14 ) ) ;
#5644 = EDGE_CURVE ( 'NONE', #1356, #5699, #3055, .T. ) ;
#5645 = DIRECTION ( 'NONE',  ( 0.000000000000000000, 0.000000000000000000, 1.000000000000000000 ) ) ;
#5646 = CARTESIAN_POINT ( 'NONE',  ( -28.87459861216645862, 60.99999999999999289, -14.47678174684361352 ) ) ;
#5647 = ORIENTED_EDGE ( 'NONE', *, *, #3352, .T. ) ;
#5648 = DIRECTION ( 'NONE',  ( -1.000000000000000000, -0.000000000000000000, -0.000000000000000000 ) ) ;
#5649 = ORIENTED_EDGE ( 'NONE', *, *, #5948, .T. ) ;
#5650 = EDGE_LOOP ( 'NONE', ( #8305, #1388, #796, #6943 ) ) ;
#5651 = CARTESIAN_POINT ( 'NONE',  ( 33.06426808735053413, 59.89212256466219486, 8.062309845534588959 ) ) ;
#5652 = ORIENTED_EDGE ( 'NONE', *, *, #3114, .T. ) ;
#5653 = CARTESIAN_POINT ( 'NONE',  ( -5.536480372579049458, -5.071221366488331661, 38.69702195666404521 ) ) ;
#5654 = EDGE_CURVE ( 'NONE', #504, #6089, #7902, .T. ) ;
#5655 = FACE_OUTER_BOUND ( 'NONE', #815, .T. ) ;
#5656 = EDGE_CURVE ( 'NONE', #1193, #3167, #4247, .T. ) ;
#5657 = EDGE_CURVE ( 'NONE', #8683, #7884, #7098, .T. ) ;
#5658 = ORIENTED_EDGE ( 'NONE', *, *, #8395, .F. ) ;
#5659 = FACE_OUTER_BOUND ( 'NONE', #2024, .T. ) ;
#5660 = EDGE_LOOP ( 'NONE', ( #9283, #2577 ) ) ;
#5661 = PLANE ( 'NONE',  #8068 ) ;
#5662 = CYLINDRICAL_SURFACE ( 'NONE', #270, 2.500000000000002220 ) ;
#5663 = CARTESIAN_POINT ( 'NONE',  ( 1.300000000000000044, -1.082531754730548190, 0.6250000000000000000 ) ) ;
#5664 = CARTESIAN_POINT ( 'NONE',  ( 12.40150588385810515, 8.712168704539934083, 36.97588844760274895 ) ) ;
#5665 = CARTESIAN_POINT ( 'NONE',  ( 23.54759692749571443, 59.99999999999999289, -18.58791755254457811 ) ) ;
#5666 = DIRECTION ( 'NONE',  ( -0.000000000000000000, -0.5000000000000002220, 0.8660254037844384856 ) ) ;
#5667 = DIRECTION ( 'NONE',  ( 1.820952055660014662E-28, 1.000000000000000000, 7.038118388768679669E-30 ) ) ;
#5668 = EDGE_LOOP ( 'NONE', ( #7409, #4714, #8742, #8283, #2494 ) ) ;
#5669 = LINE ( 'NONE', #339, #3155 ) ;
#5670 = FACE_OUTER_BOUND ( 'NONE', #5512, .T. ) ;
#5671 = ORIENTED_EDGE ( 'NONE', *, *, #6544, .T. ) ;
#5672 = DIRECTION ( 'NONE',  ( 0.000000000000000000, -0.000000000000000000, -1.000000000000000000 ) ) ;
#5673 = EDGE_LOOP ( 'NONE', ( #7278, #8290, #7882, #9641, #4545, #8058, #6154, #6909, #3660 ) ) ;
#5674 = CARTESIAN_POINT ( 'NONE',  ( -28.33333333333344939, 59.99999999999999289, 9.860132971832396009 ) ) ;
#5675 = LINE ( 'NONE', #3250, #7776 ) ;
#5676 = CARTESIAN_POINT ( 'NONE',  ( 0.000000000000000000, 28.99999999999997158, -29.00000000000000355 ) ) ;
#5677 = AXIS2_PLACEMENT_3D ( 'NONE', #7687, #3421, #5421 ) ;
#5678 = AXIS2_PLACEMENT_3D ( 'NONE', #2677, #9464, #1942 ) ;
#5679 = FACE_OUTER_BOUND ( 'NONE', #604, .T. ) ;
#5680 = ORIENTED_EDGE ( 'NONE', *, *, #8991, .F. ) ;
#5681 = DIRECTION ( 'NONE',  ( 1.735493991486226532E-29, 0.000000000000000000, -1.000000000000000000 ) ) ;
#5682 = CARTESIAN_POINT ( 'NONE',  ( -7.625823958607668374, -7.198980154853257929, 38.46531392912545755 ) ) ;
#5683 = EDGE_LOOP ( 'NONE', ( #4233, #6471, #9463, #7909, #4812 ) ) ;
#5684 = VECTOR ( 'NONE', #6289, 1000.000000000000000 ) ;
#5685 = CARTESIAN_POINT ( 'NONE',  ( 0.000000000000000000, 28.99999999999997158, 29.00000000000000355 ) ) ;
#5686 = CARTESIAN_POINT ( 'NONE',  ( -23.54469556655647722, 54.99999999999999289, -29.82695610816121956 ) ) ;
#5687 = CARTESIAN_POINT ( 'NONE',  ( 2.632839041009112258, 12.96455383109111814, 43.83318083222629014 ) ) ;
#5688 = AXIS2_PLACEMENT_3D ( 'NONE', #5944, #8966, #1700 ) ;
#5689 = VERTEX_POINT ( 'NONE', #8041 ) ;
#5690 = CARTESIAN_POINT ( 'NONE',  ( 0.000000000000000000, -0.7216878364870317197, -1.250000000000000000 ) ) ;
#5691 = ORIENTED_EDGE ( 'NONE', *, *, #9460, .T. ) ;
#5692 = DIRECTION ( 'NONE',  ( 0.000000000000000000, 0.000000000000000000, -1.000000000000000000 ) ) ;
#5693 = ORIENTED_EDGE ( 'NONE', *, *, #8313, .T. ) ;
#5694 = VERTEX_POINT ( 'NONE', #5720 ) ;
#5695 = EDGE_CURVE ( 'NONE', #5165, #8947, #2647, .T. ) ;
#5696 = CARTESIAN_POINT ( 'NONE',  ( -7.754730899493599061, -3.063035541202936418, 38.35473839958616793 ) ) ;
#5697 = DIRECTION ( 'NONE',  ( 0.000000000000000000, 0.000000000000000000, -1.000000000000000000 ) ) ;
#5698 = DIRECTION ( 'NONE',  ( -1.000000000000000000, -0.000000000000000000, -0.000000000000000000 ) ) ;
#5699 = VERTEX_POINT ( 'NONE', #3492 ) ;
#5700 = DIRECTION ( 'NONE',  ( -1.000000000000000000, 0.000000000000000000, 0.000000000000000000 ) ) ;
#5701 = CARTESIAN_POINT ( 'NONE',  ( -3.060768115627992003, 59.99034304420147379, 33.21665709534246957 ) ) ;
#5702 = ORIENTED_EDGE ( 'NONE', *, *, #9582, .F. ) ;
#5703 = LINE ( 'NONE', #482, #4959 ) ;
#5704 = EDGE_CURVE ( 'NONE', #5699, #64, #1134, .T. ) ;
#5705 = EDGE_CURVE ( 'NONE', #7606, #874, #6993, .T. ) ;
#5706 = DIRECTION ( 'NONE',  ( 0.000000000000000000, 0.000000000000000000, 1.000000000000000000 ) ) ;
#5707 = LINE ( 'NONE', #9511, #1281 ) ;
#5708 = FACE_OUTER_BOUND ( 'NONE', #9529, .T. ) ;
#5709 = AXIS2_PLACEMENT_3D ( 'NONE', #2185, #6041, #7638 ) ;
#5710 = EDGE_CURVE ( 'NONE', #1760, #6269, #7849, .T. ) ;
#5711 = DIRECTION ( 'NONE',  ( -0.000000000000000000, -0.000000000000000000, 1.000000000000000000 ) ) ;
#5712 = AXIS2_PLACEMENT_3D ( 'NONE', #7574, #73, #3162 ) ;
#5713 = ORIENTED_EDGE ( 'NONE', *, *, #868, .T. ) ;
#5714 = DIRECTION ( 'NONE',  ( 0.9449569463147374782, 0.000000000000000000, 0.3271946967961527619 ) ) ;
#5715 = FACE_OUTER_BOUND ( 'NONE', #8207, .T. ) ;
#5716 = ORIENTED_EDGE ( 'NONE', *, *, #1533, .T. ) ;
#5717 = CARTESIAN_POINT ( 'NONE',  ( 5.423418723394456162E-28, -2.066522830327504070E-28, -26.00000000000004974 ) ) ;
#5718 = CARTESIAN_POINT ( 'NONE',  ( 1.636886378333599496E-26, 78.08723716182652197, -37.00000000000000711 ) ) ;
#5719 = EDGE_CURVE ( 'NONE', #9428, #2716, #5860, .T. ) ;
#5720 = CARTESIAN_POINT ( 'NONE',  ( -5.371095444502437921, 60.99999999999999289, -34.07933880998933773 ) ) ;
#5721 = VECTOR ( 'NONE', #8042, 1000.000000000000000 ) ;
#5722 = DIRECTION ( 'NONE',  ( 1.735493991486225972E-29, -6.508102468073347395E-30, -1.000000000000000000 ) ) ;
#5723 = AXIS2_PLACEMENT_3D ( 'NONE', #5059, #8861, #9747 ) ;
#5724 = DIRECTION ( 'NONE',  ( 0.000000000000000000, 0.000000000000000000, 1.000000000000000000 ) ) ;
#5725 = VECTOR ( 'NONE', #8836, 1000.000000000000000 ) ;
#5726 = EDGE_LOOP ( 'NONE', ( #6134, #6213, #6712, #8549, #3609, #7468, #6615, #747, #1401, #9604, #935, #5310, #1130, #703, #88, #3094 ) ) ;
#5727 = FACE_BOUND ( 'NONE', #8955, .T. ) ;
#5728 = CARTESIAN_POINT ( 'NONE',  ( -2.808770322584149604, -15.00000000000000000, 29.89902100188472645 ) ) ;
#5729 = AXIS2_PLACEMENT_3D ( 'NONE', #2591, #4194, #8492 ) ;
#5730 = VERTEX_POINT ( 'NONE', #9753 ) ;
#5731 = CARTESIAN_POINT ( 'NONE',  ( 8.677469957431129860E-27, 45.50000000000019185, -26.00000000000014566 ) ) ;
#5732 = LINE ( 'NONE', #2564, #8288 ) ;
#5733 = CARTESIAN_POINT ( 'NONE',  ( 5.037425304447057606, 11.93964564789587790, 43.34856681498735043 ) ) ;
#5734 = ORIENTED_EDGE ( 'NONE', *, *, #5757, .T. ) ;
#5735 = DIRECTION ( 'NONE',  ( 1.735493991486225972E-29, -6.508102468073347395E-30, -1.000000000000000000 ) ) ;
#5736 = ORIENTED_EDGE ( 'NONE', *, *, #8975, .F. ) ;
#5737 = CARTESIAN_POINT ( 'NONE',  ( 0.000000000000000000, -50.91168824543140659, 17.99999999999999645 ) ) ;
#5738 = EDGE_LOOP ( 'NONE', ( #3049, #1250, #6906, #863 ) ) ;
#5739 = ADVANCED_FACE ( 'NONE', ( #5998 ), #4338, .T. ) ;
#5740 = ORIENTED_EDGE ( 'NONE', *, *, #9263, .T. ) ;
#5741 = CARTESIAN_POINT ( 'NONE',  ( 0.01843853347452210911, 13.29483547765103069, 43.99999130734106245 ) ) ;
#5742 = VECTOR ( 'NONE', #6626, 1000.000000000000000 ) ;
#5743 = CARTESIAN_POINT ( 'NONE',  ( -33.06426808735054124, 49.99999999999999289, -3.062309845534580077 ) ) ;
#5744 = CARTESIAN_POINT ( 'NONE',  ( -8.545448575588393325, 44.50000000000019185, -24.55555555555569569 ) ) ;
#5745 = AXIS2_PLACEMENT_3D ( 'NONE', #8738, #3400, #8786 ) ;
#5746 = AXIS2_PLACEMENT_3D ( 'NONE', #7742, #6939, #9232 ) ;
#5747 = ORIENTED_EDGE ( 'NONE', *, *, #2851, .T. ) ;
#5748 = DIRECTION ( 'NONE',  ( 0.000000000000000000, 0.000000000000000000, 1.000000000000000000 ) ) ;
#5749 = ORIENTED_EDGE ( 'NONE', *, *, #5502, .F. ) ;
#5750 = VERTEX_POINT ( 'NONE', #633 ) ;
#5751 = DIRECTION ( 'NONE',  ( -0.000000000000000000, -1.000000000000000000, -0.000000000000000000 ) ) ;
#5752 = CARTESIAN_POINT ( 'NONE',  ( 2.400000000000000799, 2.694222958124176513E-16, -2.199999999999999734 ) ) ;
#5753 = VECTOR ( 'NONE', #7285, 1000.000000000000000 ) ;
#5754 = DIRECTION ( 'NONE',  ( 0.000000000000000000, 0.000000000000000000, -1.000000000000000000 ) ) ;
#5755 = EDGE_CURVE ( 'NONE', #9184, #1828, #8979, .T. ) ;
#5756 = CYLINDRICAL_SURFACE ( 'NONE', #4746, 2.499999999999998668 ) ;
#5757 = EDGE_CURVE ( 'NONE', #4378, #1718, #2188, .T. ) ;
#5758 = CARTESIAN_POINT ( 'NONE',  ( 0.000000000000000000, 30.00000000000000000, 0.000000000000000000 ) ) ;
#5759 = AXIS2_PLACEMENT_3D ( 'NONE', #5297, #855, #8309 ) ;
#5760 = ADVANCED_FACE ( 'NONE', ( #2150, #8143 ), #7493, .T. ) ;
#5761 = AXIS2_PLACEMENT_3D ( 'NONE', #6524, #8020, #5058 ) ;
#5762 = EDGE_CURVE ( 'NONE', #7580, #7439, #8231, .T. ) ;
#5763 = ORIENTED_EDGE ( 'NONE', *, *, #2487, .T. ) ;
#5764 = PLANE ( 'NONE',  #4226 ) ;
#5765 = CARTESIAN_POINT ( 'NONE',  ( 10.00000000000001599, 3.294852476638864491, 41.36423575989288537 ) ) ;
#5766 = EDGE_CURVE ( 'NONE', #2789, #6478, #1952, .T. ) ;
#5767 = AXIS2_PLACEMENT_3D ( 'NONE', #9395, #4067, #4807 ) ;
#5768 = EDGE_LOOP ( 'NONE', ( #4276, #2840, #2759, #3698, #2971, #8896, #513, #3030, #5969, #2136, #4072, #7470, #4223, #2814, #3466, #134 ) ) ;
#5769 = CARTESIAN_POINT ( 'NONE',  ( -8.216777476527294510, 53.50000000000031264, -23.61111111111107519 ) ) ;
#5770 =( NAMED_UNIT ( * ) PLANE_ANGLE_UNIT ( ) SI_UNIT ( $, .RADIAN. ) );
#5771 = TOROIDAL_SURFACE ( 'NONE', #1507, 37.00000000000000711, 3.000000000000002665 ) ;
#5772 = FACE_OUTER_BOUND ( 'NONE', #4755, .T. ) ;
#5773 = AXIS2_PLACEMENT_3D ( 'NONE', #92, #4536, #9715 ) ;
#5774 = CARTESIAN_POINT ( 'NONE',  ( -6.000000000000005329, -10.00000000000000533, -26.32489316217636954 ) ) ;
#5775 = EDGE_CURVE ( 'NONE', #2914, #9233, #3037, .T. ) ;
#5776 = EDGE_CURVE ( 'NONE', #4788, #71, #1021, .T. ) ;
#5777 = CIRCLE ( 'NONE', #2772, 19.00000000000005684 ) ;
#5778 = EDGE_CURVE ( 'NONE', #7854, #4551, #1333, .T. ) ;
#5779 = EDGE_LOOP ( 'NONE', ( #6275, #153 ) ) ;
#5780 = PLANE ( 'NONE',  #1185 ) ;
#5781 = VERTEX_POINT ( 'NONE', #2053 ) ;
#5782 = LINE ( 'NONE', #6455, #6975 ) ;
#5783 = CARTESIAN_POINT ( 'NONE',  ( -8.329014317829159353, -6.778170143341801790, 38.25993911327689290 ) ) ;
#5784 = ORIENTED_EDGE ( 'NONE', *, *, #574, .F. ) ;
#5785 = AXIS2_PLACEMENT_3D ( 'NONE', #1091, #6318, #4756 ) ;
#5786 = DIRECTION ( 'NONE',  ( -0.000000000000000000, -1.000000000000000000, -0.000000000000000000 ) ) ;
#5787 = PLANE ( 'NONE',  #8131 ) ;
#5788 = CARTESIAN_POINT ( 'NONE',  ( 3.885102854800722483, 12.53650132828193797, 38.86177049418535034 ) ) ;
#5789 = DIRECTION ( 'NONE',  ( 0.000000000000000000, -1.000000000000000000, 0.000000000000000000 ) ) ;
#5790 = VERTEX_POINT ( 'NONE', #7447 ) ;
#5791 = CARTESIAN_POINT ( 'NONE',  ( -33.72911585420148128, 59.92558239856793278, -3.146586008005425761 ) ) ;
#5792 = CARTESIAN_POINT ( 'NONE',  ( 33.06426808735054124, 60.99999999999999289, 1.062309845534581632 ) ) ;
#5793 = DIRECTION ( 'NONE',  ( 0.000000000000000000, 0.000000000000000000, -1.000000000000000000 ) ) ;
#5794 = ORIENTED_EDGE ( 'NONE', *, *, #107, .F. ) ;
#5795 = ORIENTED_EDGE ( 'NONE', *, *, #2672, .T. ) ;
#5796 = CARTESIAN_POINT ( 'NONE',  ( -8.116472182054980777, 9.145332620307328853, 42.28305399575716450 ) ) ;
#5797 = EDGE_CURVE ( 'NONE', #1718, #9349, #7487, .T. ) ;
#5798 = DIRECTION ( 'NONE',  ( 0.000000000000000000, 0.000000000000000000, 1.000000000000000000 ) ) ;
#5799 = LINE ( 'NONE', #5840, #532 ) ;
#5800 = ORIENTED_EDGE ( 'NONE', *, *, #8959, .T. ) ;
#5801 = CARTESIAN_POINT ( 'NONE',  ( 31.00000000000000711, -15.00000000000000000, 6.000000000000000000 ) ) ;
#5802 = ORIENTED_EDGE ( 'NONE', *, *, #3586, .F. ) ;
#5803 = ORIENTED_EDGE ( 'NONE', *, *, #5695, .T. ) ;
#5804 = CARTESIAN_POINT ( 'NONE',  ( 31.00000000000000711, 27.42469319230601243, 6.000000000000000000 ) ) ;
#5805 = CARTESIAN_POINT ( 'NONE',  ( -31.00000000000000711, 27.42469319230601243, -5.999999999999996447 ) ) ;
#5806 = CARTESIAN_POINT ( 'NONE',  ( 12.50302036141013140, 8.406344128993804787, 36.94162958640247751 ) ) ;
#5807 = PLANE ( 'NONE',  #7584 ) ;
#5808 = APPLICATION_CONTEXT ( 'automotive_design' ) ;
#5809 = ADVANCED_FACE ( 'NONE', ( #8089 ), #4396, .T. ) ;
#5810 = CARTESIAN_POINT ( 'NONE',  ( -5.000000000000006217, 30.00000000000000000, -25.51470164434615029 ) ) ;
#5811 = ORIENTED_EDGE ( 'NONE', *, *, #74, .F. ) ;
#5812 = CARTESIAN_POINT ( 'NONE',  ( 0.000000000000000000, 30.00000000000000000, 0.000000000000000000 ) ) ;
#5813 = CARTESIAN_POINT ( 'NONE',  ( 10.00000000000009948, 3.626867479774634084, 41.36423575989284274 ) ) ;
#5814 = VERTEX_POINT ( 'NONE', #3639 ) ;
#5815 = FACE_OUTER_BOUND ( 'NONE', #4024, .T. ) ;
#5816 = CARTESIAN_POINT ( 'NONE',  ( -13.15959852261851815, 1.059259259969981937, 36.71292293559446307 ) ) ;
#5817 = CARTESIAN_POINT ( 'NONE',  ( -8.216777476527294510, 50.00000000000032685, -23.61111111111111427 ) ) ;
#5818 = VECTOR ( 'NONE', #9605, 1000.000000000000000 ) ;
#5819 = LINE ( 'NONE', #2845, #4811 ) ;
#5820 = ORIENTED_EDGE ( 'NONE', *, *, #4492, .T. ) ;
#5821 = LINE ( 'NONE', #2059, #683 ) ;
#5822 = CARTESIAN_POINT ( 'NONE',  ( -0.4572298495115817429, -15.00000000000015987, 36.76400391796496336 ) ) ;
#5823 = ORIENTED_EDGE ( 'NONE', *, *, #166, .T. ) ;
#5824 = EDGE_CURVE ( 'NONE', #9481, #2330, #3104, .T. ) ;
#5825 = EDGE_CURVE ( 'NONE', #167, #2908, #3941, .T. ) ;
#5826 = EDGE_CURVE ( 'NONE', #8835, #7681, #2261, .T. ) ;
#5827 = CARTESIAN_POINT ( 'NONE',  ( 5.562309845534588959, 59.99999999999999289, -35.56426808735054834 ) ) ;
#5828 = AXIS2_PLACEMENT_3D ( 'NONE', #3796, #9086, #2302 ) ;
#5829 = AXIS2_PLACEMENT_3D ( 'NONE', #8576, #1855, #7692 ) ;
#5830 = DIRECTION ( 'NONE',  ( -0.000000000000000000, 1.000000000000000000, -0.000000000000000000 ) ) ;
#5831 = CARTESIAN_POINT ( 'NONE',  ( 10.01906723522320064, 13.16737651941478049, 37.69215544616801594 ) ) ;
#5832 = EDGE_LOOP ( 'NONE', ( #2121, #6617, #7921, #8441 ) ) ;
#5833 = DIRECTION ( 'NONE',  ( -1.533293416683393860E-16, 0.7071067811865376918, -0.7071067811865573427 ) ) ;
#5834 = EDGE_LOOP ( 'NONE', ( #8628, #8795, #2640, #4225, #6911 ) ) ;
#5835 = CARTESIAN_POINT ( 'NONE',  ( 9.815840903884561541, 39.99999999999999289, -28.34870838944214100 ) ) ;
#5836 = VERTEX_POINT ( 'NONE', #9230 ) ;
#5837 = DIRECTION ( 'NONE',  ( -0.000000000000000000, 1.000000000000000000, -0.000000000000000000 ) ) ;
#5838 = ORIENTED_EDGE ( 'NONE', *, *, #9280, .F. ) ;
#5839 = CARTESIAN_POINT ( 'NONE',  ( 0.000000000000000000, 54.99999999999999289, 0.000000000000000000 ) ) ;
#5840 = CARTESIAN_POINT ( 'NONE',  ( 9.762153702110021092E-27, 50.50000000000031974, -25.00000000000000000 ) ) ;
#5841 = SHAPE_REPRESENTATION ( 'MAS-312', ( #2378, #9007, #6463, #4752, #3004, #347, #9645, #8703, #5392, #4608, #8860, #2203 ), #6481 ) ;
#5842 = CIRCLE ( 'NONE', #6307, 38.00000000000000711 ) ;
#5843 = ORIENTED_EDGE ( 'NONE', *, *, #8735, .F. ) ;
#5844 = CYLINDRICAL_SURFACE ( 'NONE', #4439, 27.99999999999999289 ) ;
#5845 = VERTEX_POINT ( 'NONE', #196 ) ;
#5846 = CARTESIAN_POINT ( 'NONE',  ( -8.545448575588375562, 55.00000000000030553, -24.55555555555558911 ) ) ;
#5847 = DIRECTION ( 'NONE',  ( 0.000000000000000000, 0.000000000000000000, -1.000000000000000000 ) ) ;
#5848=STYLED_ITEM('',(#9806),#9647);
#5849 =( LENGTH_UNIT ( ) NAMED_UNIT ( * ) SI_UNIT ( .MILLI., .METRE. ) );
#5850 = DIRECTION ( 'NONE',  ( -1.820952055660014662E-28, -1.000000000000000000, -7.038118388768679669E-30 ) ) ;
#5851 = CARTESIAN_POINT ( 'NONE',  ( -33.06426808735054124, 49.99999999999999289, -8.062309845534583630 ) ) ;
#5852 = VECTOR ( 'NONE', #6783, 1000.000000000000000 ) ;
#5853 = PRODUCT_DEFINITION_FORMATION_WITH_SPECIFIED_SOURCE ( 'ANY', '', #786, .NOT_KNOWN. ) ;
#5854 = LINE ( 'NONE', #3631, #9620 ) ;
#5855 = VERTEX_POINT ( 'NONE', #8434 ) ;
#5856 = DIRECTION ( 'NONE',  ( -1.820952055660014662E-28, -1.000000000000000000, 6.508102468073347395E-30 ) ) ;
#5857 = CARTESIAN_POINT ( 'NONE',  ( 5.326140061663600100, 11.76457241320986924, 43.27053568042958887 ) ) ;
#5858 = DIRECTION ( 'NONE',  ( 1.735493991486225972E-29, -6.508102468073347395E-30, -1.000000000000000000 ) ) ;
#5859 = SURFACE_STYLE_FILL_AREA ( #4198 ) ;
#5860 = LINE ( 'NONE', #3595, #7964 ) ;
#5861 = AXIS2_PLACEMENT_3D ( 'NONE', #8653, #4116, #9296 ) ;
#5862 = FACE_OUTER_BOUND ( 'NONE', #1384, .T. ) ;
#5863 = VERTEX_POINT ( 'NONE', #3283 ) ;
#5864 = DIRECTION ( 'NONE',  ( 0.000000000000000000, 1.000000000000000000, 0.000000000000000000 ) ) ;
#5865 = CARTESIAN_POINT ( 'NONE',  ( -3.910602396084473575, -8.894839577748838266, 39.26794276223228053 ) ) ;
#5866 = AXIS2_PLACEMENT_3D ( 'NONE', #985, #4844, #6408 ) ;
#5867 = ORIENTED_EDGE ( 'NONE', *, *, #1088, .F. ) ;
#5868 = CARTESIAN_POINT ( 'NONE',  ( 24.67792535850613334, 30.00000000000000000, -4.000000000000006217 ) ) ;
#5869 = DIRECTION ( 'NONE',  ( -1.000000000000000000, -0.000000000000000000, -0.000000000000000000 ) ) ;
#5870 = ORIENTED_EDGE ( 'NONE', *, *, #3455, .T. ) ;
#5871 = VECTOR ( 'NONE', #8906, 1000.000000000000000 ) ;
#5872 = VECTOR ( 'NONE', #2401, 1000.000000000000000 ) ;
#5873 = CARTESIAN_POINT ( 'NONE',  ( 4.720363748491940292, 12.14410912167428869, 38.78759026100516394 ) ) ;
#5874 = EDGE_CURVE ( 'NONE', #5016, #2330, #5519, .T. ) ;
#5875 = EDGE_LOOP ( 'NONE', ( #5802, #6590, #2228, #9726 ) ) ;
#5876 = DIRECTION ( 'NONE',  ( -1.820952055660014662E-28, -1.000000000000000000, -7.038118388768679669E-30 ) ) ;
#5877 = ADVANCED_FACE ( 'NONE', ( #8338 ), #1713, .F. ) ;
#5878 = FACE_OUTER_BOUND ( 'NONE', #5891, .T. ) ;
#5879 = CARTESIAN_POINT ( 'NONE',  ( 1.138917931912835794E-26, 56.00000000000030553, -25.00000000000000000 ) ) ;
#5880 = ORIENTED_EDGE ( 'NONE', *, *, #4987, .F. ) ;
#5881 = CARTESIAN_POINT ( 'NONE',  ( -33.06426808735054124, 60.99999999999999289, -5.562309845534586294 ) ) ;
#5882 = VERTEX_POINT ( 'NONE', #3237 ) ;
#5883 = CARTESIAN_POINT ( 'NONE',  ( -9.686515203225052772, 13.58116064233279552, 37.77923906255211506 ) ) ;
#5884 = DIRECTION ( 'NONE',  ( 0.000000000000000000, 0.000000000000000000, 1.000000000000000000 ) ) ;
#5885 = DIRECTION ( 'NONE',  ( 0.3286710990610922090, 6.289316826390952918E-29, 0.9444444444444435316 ) ) ;
#5886 = ADVANCED_FACE ( 'NONE', ( #149 ), #1621, .F. ) ;
#5887 = ORIENTED_EDGE ( 'NONE', *, *, #1124, .T. ) ;
#5888 = DIRECTION ( 'NONE',  ( -0.000000000000000000, -1.000000000000000000, -0.000000000000000000 ) ) ;
#5889 = EDGE_CURVE ( 'NONE', #9126, #9742, #5329, .T. ) ;
#5890 = ORIENTED_EDGE ( 'NONE', *, *, #9744, .F. ) ;
#5891 = EDGE_LOOP ( 'NONE', ( #4817, #5480, #391, #4893, #2312 ) ) ;
#5892 = CARTESIAN_POINT ( 'NONE',  ( -5.000000000000006217, 30.00000000000000000, -30.00000000000000711 ) ) ;
#5893 = DIRECTION ( 'NONE',  ( -1.820952055660014662E-28, -1.000000000000000000, 6.508102468073347395E-30 ) ) ;
#5894 = CARTESIAN_POINT ( 'NONE',  ( 0.000000000000000000, 59.99999999999999289, -30.00000000000000711 ) ) ;
#5895 = FILL_AREA_STYLE ('',( #9657 ) ) ;
#5896 = CIRCLE ( 'NONE', #3693, 5.000000000000001776 ) ;
#5897 = DIRECTION ( 'NONE',  ( -0.7849198975831889191, -0.000000000000000000, 0.6195972517514874989 ) ) ;
#5898 = VERTEX_POINT ( 'NONE', #6105 ) ;
#5899 = CIRCLE ( 'NONE', #8437, 40.00000000000000711 ) ;
#5900 = CARTESIAN_POINT ( 'NONE',  ( -8.871504613779674031, 62.00000000000265743, 36.13240710991937021 ) ) ;
#5901 = LINE ( 'NONE', #7394, #8001 ) ;
#5902 = CARTESIAN_POINT ( 'NONE',  ( 20.99999999999999645, 28.99999999999997158, -4.000000000000006217 ) ) ;
#5903 = CARTESIAN_POINT ( 'NONE',  ( 1.773930110362821555, -15.00000000000000178, 30.27515255412638240 ) ) ;
#5904 = CARTESIAN_POINT ( 'NONE',  ( 10.84614626901583634, 59.99999999999999289, 31.16666666666671759 ) ) ;
#5905 = CARTESIAN_POINT ( 'NONE',  ( -4.424613605680260520, 17.45796735942974109, 38.75301155415253618 ) ) ;
#5906 = EDGE_CURVE ( 'NONE', #3718, #4111, #2106, .T. ) ;
#5907 = AXIS2_PLACEMENT_3D ( 'NONE', #4612, #5968, #4659 ) ;
#5908 = VECTOR ( 'NONE', #3678, 1000.000000000000341 ) ;
#5909 = CIRCLE ( 'NONE', #2446, 1.500000000000003109 ) ;
#5910 = DIRECTION ( 'NONE',  ( 0.9860132971832693549, 1.788557213313974126E-28, -0.1666666666666657970 ) ) ;
#5911 = AXIS2_PLACEMENT_3D ( 'NONE', #8661, #4173, #5692 ) ;
#5912 = AXIS2_PLACEMENT_3D ( 'NONE', #5265, #2291, #2093 ) ;
#5913 = EDGE_LOOP ( 'NONE', ( #6603, #2468 ) ) ;
#5914 = DIRECTION ( 'NONE',  ( 2.168404344971006649E-16, 0.000000000000000000, 1.000000000000000000 ) ) ;
#5915 = CARTESIAN_POINT ( 'NONE',  ( 10.67347934733978754, -5.256592221152843969, 37.51339085603135004 ) ) ;
#5916 = ORIENTED_EDGE ( 'NONE', *, *, #8248, .F. ) ;
#5917 = LINE ( 'NONE', #4359, #2391 ) ;
#5918 = AXIS2_PLACEMENT_3D ( 'NONE', #96, #3085, #5425 ) ;
#5919 = AXIS2_PLACEMENT_3D ( 'NONE', #1140, #4800, #2410 ) ;
#5920 = CARTESIAN_POINT ( 'NONE',  ( 0.000000000000000000, 0.000000000000000000, 0.000000000000000000 ) ) ;
#5921 = ORIENTED_EDGE ( 'NONE', *, *, #224, .T. ) ;
#5922 = CARTESIAN_POINT ( 'NONE',  ( 9.601051617431352270, 6.203770162293365864, 37.95839508490225711 ) ) ;
#5923 = SHAPE_DEFINITION_REPRESENTATION ( #4738, #5213 ) ;
#5924 = EDGE_CURVE ( 'NONE', #6645, #5153, #8529, .T. ) ;
#5925 = ORIENTED_EDGE ( 'NONE', *, *, #9158, .F. ) ;
#5926 = CARTESIAN_POINT ( 'NONE',  ( -34.95336322954870667, 59.50565096299369827, -3.917041198934857693 ) ) ;
#5927 = TOROIDAL_SURFACE ( 'NONE', #2301, 33.00000000000000711, 5.000000000000000000 ) ;
#5928 = VERTEX_POINT ( 'NONE', #6151 ) ;
#5929 = CARTESIAN_POINT ( 'NONE',  ( 34.60286690457041914, 59.67177527313210561, 3.585274540811282051 ) ) ;
#5930 = ORIENTED_EDGE ( 'NONE', *, *, #983, .T. ) ;
#5931 = FACE_OUTER_BOUND ( 'NONE', #9348, .T. ) ;
#5932 = EDGE_LOOP ( 'NONE', ( #9186, #8422, #2875, #4161, #3647, #6278, #5264 ) ) ;
#5933 = CARTESIAN_POINT ( 'NONE',  ( -1.294388769339064327, 13.21620364998245023, 43.95989878156864705 ) ) ;
#5934 = B_SPLINE_CURVE_WITH_KNOTS ( 'NONE', 3,
 ( #8499, #4153, #4056, #9437, #7101, #4103, #9288, #2649, #349, #6260, #1137, #4747, #400, #5534, #3353, #3405, #9380, #7046 ),
 .UNSPECIFIED., .F., .F.,
 ( 4, 2, 2, 2, 2, 2, 2, 2, 4 ),
 ( 0.003057178249550605680, 0.003880613475145725487, 0.004704048700740845294, 0.005527483926335964234, 0.006350919151931084042, 0.007174354377526204717, 0.007997789603121323657, 0.008821224828716443464, 0.009644660054311565006 ),
 .UNSPECIFIED. ) ;
#5935 = CARTESIAN_POINT ( 'NONE',  ( 0.000000000000000000, 0.000000000000000000, 3.799999999999999378 ) ) ;
#5936 = EDGE_CURVE ( 'NONE', #9170, #3887, #5481, .T. ) ;
#5937 = LINE ( 'NONE', #5976, #3355 ) ;
#5938 = VERTEX_POINT ( 'NONE', #9133 ) ;
#5939 = CARTESIAN_POINT ( 'NONE',  ( 5.371095444502685723, 61.99999999999999289, 34.07933880998929510 ) ) ;
#5940 = CARTESIAN_POINT ( 'NONE',  ( 33.06426808735054124, 61.99999999999999289, 5.562309845534586294 ) ) ;
#5941 = ORIENTED_EDGE ( 'NONE', *, *, #273, .F. ) ;
#5942 = CARTESIAN_POINT ( 'NONE',  ( 1.257247067695987565E-26, 60.00000000000029843, -37.00000000000000711 ) ) ;
#5943 =( NAMED_UNIT ( * ) PLANE_ANGLE_UNIT ( ) SI_UNIT ( $, .RADIAN. ) );
#5944 = CARTESIAN_POINT ( 'NONE',  ( 0.000000000000000000, 39.99999999999999289, 0.000000000000000000 ) ) ;
#5945 = EDGE_CURVE ( 'NONE', #3216, #9301, #7740, .T. ) ;
#5946 = CARTESIAN_POINT ( 'NONE',  ( 25.90235662024523577, 54.99999999999999289, -20.44670930779909312 ) ) ;
#5947 = EDGE_CURVE ( 'NONE', #1652, #9574, #6059, .T. ) ;
#5948 = EDGE_CURVE ( 'NONE', #8562, #5205, #405, .T. ) ;
#5949 = FACE_OUTER_BOUND ( 'NONE', #7062, .T. ) ;
#5950 = ORIENTED_EDGE ( 'NONE', *, *, #8842, .F. ) ;
#5951 = CARTESIAN_POINT ( 'NONE',  ( 7.522530930366955637, -3.325240747455041834, 42.53435141087333449 ) ) ;
#5952 = DIRECTION ( 'NONE',  ( 0.000000000000000000, 0.000000000000000000, 1.000000000000000000 ) ) ;
#5953 = CYLINDRICAL_SURFACE ( 'NONE', #3174, 17.99999999999999645 ) ;
#5954 = CARTESIAN_POINT ( 'NONE',  ( 2.008133409164431615, 27.99999999999992184, -31.00000000000000711 ) ) ;
#5955 = CARTESIAN_POINT ( 'NONE',  ( 0.000000000000000000, -4.999999999999999112, 0.000000000000000000 ) ) ;
#5956 = DIRECTION ( 'NONE',  ( 1.735493991486225692E-29, -6.508102468073347395E-30, -1.000000000000000000 ) ) ;
#5957 = ORIENTED_EDGE ( 'NONE', *, *, #6948, .T. ) ;
#5958 = DIRECTION ( 'NONE',  ( 1.000000000000000000, 0.000000000000000000, -1.084202172485503448E-16 ) ) ;
#5959 = CARTESIAN_POINT ( 'NONE',  ( 10.60693692882557038, -15.00000000000062528, 37.26904593215826367 ) ) ;
#5960 = VERTEX_POINT ( 'NONE', #2345 ) ;
#5961 = DIRECTION ( 'NONE',  ( 0.9860132971832693549, 1.788557213313974126E-28, -0.1666666666666657970 ) ) ;
#5962 = CARTESIAN_POINT ( 'NONE',  ( 33.06426808735054124, 60.99999999999999289, 1.062309845534581632 ) ) ;
#5963 = ORIENTED_EDGE ( 'NONE', *, *, #7218, .F. ) ;
#5964 = CARTESIAN_POINT ( 'NONE',  ( 9.114420836480412902, 7.422247012081075290, 41.82255323698446148 ) ) ;
#5965 = SHAPE_DEFINITION_REPRESENTATION ( #7092, #5841 ) ;
#5966 = ORIENTED_EDGE ( 'NONE', *, *, #6545, .F. ) ;
#5967 = CARTESIAN_POINT ( 'NONE',  ( -33.06426808735054124, 49.99999999999999289, -8.062309845534585406 ) ) ;
#5968 = DIRECTION ( 'NONE',  ( -0.000000000000000000, -1.000000000000000000, -0.000000000000000000 ) ) ;
#5969 = ORIENTED_EDGE ( 'NONE', *, *, #197, .F. ) ;
#5970 = DIRECTION ( 'NONE',  ( 0.000000000000000000, 0.000000000000000000, 1.000000000000000000 ) ) ;
#5971 = ORIENTED_EDGE ( 'NONE', *, *, #106, .F. ) ;
#5972 = DIRECTION ( 'NONE',  ( 0.000000000000000000, 0.000000000000000000, 1.000000000000000000 ) ) ;
#5973 = AXIS2_PLACEMENT_3D ( 'NONE', #1499, #2173, #1450 ) ;
#5974 = DIRECTION ( 'NONE',  ( 0.000000000000000000, 0.000000000000000000, -1.000000000000000000 ) ) ;
#5975 = B_SPLINE_CURVE_WITH_KNOTS ( 'NONE', 3,
 ( #3226, #9019, #6036, #875 ),
 .UNSPECIFIED., .F., .F.,
 ( 4, 4 ),
 ( 8.673617379884035472E-19, 0.006018989108141226639 ),
 .UNSPECIFIED. ) ;
#5976 = CARTESIAN_POINT ( 'NONE',  ( 5.423418723394456162E-28, -2.066522830327504070E-28, -26.00000000000006395 ) ) ;
#5977 = AXIS2_PLACEMENT_3D ( 'NONE', #1798, #4825, #1064 ) ;
#5978 = EDGE_LOOP ( 'NONE', ( #306, #8745, #993, #5658 ) ) ;
#5979 = CARTESIAN_POINT ( 'NONE',  ( -9.815840903884557989, 59.99999999999999289, 28.34870838944214455 ) ) ;
#5980 = EDGE_CURVE ( 'NONE', #6704, #8580, #4691, .T. ) ;
#5981 = ORIENTED_EDGE ( 'NONE', *, *, #1724, .F. ) ;
#5982 = ORIENTED_EDGE ( 'NONE', *, *, #4213, .T. ) ;
#5983 = CARTESIAN_POINT ( 'NONE',  ( 0.000000000000000000, -15.00000000000000000, 0.000000000000000000 ) ) ;
#5984 = SHAPE_REPRESENTATION_RELATIONSHIP ( 'NONE' , 'NONE' ,  #1483, #1270 ) ;
#5985 = DIRECTION ( 'NONE',  ( 0.000000000000000000, 0.000000000000000000, 1.000000000000000000 ) ) ;
#5986 = LINE ( 'NONE', #7437, #5908 ) ;
#5987 = AXIS2_PLACEMENT_3D ( 'NONE', #3035, #973, #2442 ) ;
#5988 = CARTESIAN_POINT ( 'NONE',  ( 2.040301830986985809, -9.344775919449732626, 39.47202367093716191 ) ) ;
#5989 = CARTESIAN_POINT ( 'NONE',  ( -4.665243217607704551, 29.66524321760768501, -25.23917843705063646 ) ) ;
#5990 = EDGE_CURVE ( 'NONE', #3624, #1910, #7696, .T. ) ;
#5991 = EDGE_CURVE ( 'NONE', #2117, #8507, #929, .T. ) ;
#5992 = ORIENTED_EDGE ( 'NONE', *, *, #35, .T. ) ;
#5993 = PLANE ( 'NONE',  #28 ) ;
#5994 = CARTESIAN_POINT ( 'NONE',  ( -8.216777476527294510, 46.00000000000018474, -23.61111111111111427 ) ) ;
#5995 = EDGE_CURVE ( 'NONE', #1637, #5928, #248, .T. ) ;
#5996 = CARTESIAN_POINT ( 'NONE',  ( 0.3582566269629631206, -15.00000000000000000, 30.57108970959263416 ) ) ;
#5997 = CARTESIAN_POINT ( 'NONE',  ( 1.221566888952841201E-22, 27.99999999999992184, -31.00000000000000711 ) ) ;
#5998 = FACE_OUTER_BOUND ( 'NONE', #5978, .T. ) ;
#5999 = EDGE_CURVE ( 'NONE', #6799, #4378, #8596, .T. ) ;
#6000 = LINE ( 'NONE', #4491, #1327 ) ;
#6001 = EDGE_CURVE ( 'NONE', #4765, #7319, #4975, .T. ) ;
#6002 = VERTEX_POINT ( 'NONE', #4091 ) ;
#6003 = CARTESIAN_POINT ( 'NONE',  ( 0.000000000000000000, 30.99999999999998579, -40.00000000000000711 ) ) ;
#6004 = CARTESIAN_POINT ( 'NONE',  ( 4.909944792989705320, -8.520966008424666782, 39.09496844136518945 ) ) ;
#6005 = ORIENTED_EDGE ( 'NONE', *, *, #8452, .F. ) ;
#6006 = AXIS2_PLACEMENT_3D ( 'NONE', #696, #4999, #9535 ) ;
#6007 = VECTOR ( 'NONE', #330, 1000.000000000000114 ) ;
#6008 = CARTESIAN_POINT ( 'NONE',  ( 0.000000000000000000, 58.99999999999999289, 0.000000000000000000 ) ) ;
#6009 = CARTESIAN_POINT ( 'NONE',  ( 8.369359826574806283E-27, 46.00000000000018474, 2.927413515468598497E-28 ) ) ;
#6010 = EDGE_LOOP ( 'NONE', ( #7955, #2367, #562 ) ) ;
#6011 = CARTESIAN_POINT ( 'NONE',  ( 8.648354992365815619, -1.736301028422764903, 42.04488899069198027 ) ) ;
#6012 = SHAPE_DEFINITION_REPRESENTATION ( #8687, #2928 ) ;
#6013 = CIRCLE ( 'NONE', #4151, 1.500000000000001332 ) ;
#6014 = VERTEX_POINT ( 'NONE', #6345 ) ;
#6015 = CARTESIAN_POINT ( 'NONE',  ( 33.06426808735054124, 69.99999999999998579, 3.062309845534584074 ) ) ;
#6016 = CYLINDRICAL_SURFACE ( 'NONE', #1415, 30.00000000000001066 ) ;
#6017 = FACE_OUTER_BOUND ( 'NONE', #4144, .T. ) ;
#6018 = ORIENTED_EDGE ( 'NONE', *, *, #1897, .F. ) ;
#6019 = CARTESIAN_POINT ( 'NONE',  ( 1.084683744678891232E-26, 56.00000000000030553, -24.09806918451524638 ) ) ;
#6020 = ORIENTED_EDGE ( 'NONE', *, *, #2441, .T. ) ;
#6021 = DIRECTION ( 'NONE',  ( -0.000000000000000000, 1.000000000000000000, -0.000000000000000000 ) ) ;
#6022 = LINE ( 'NONE', #3816, #6493 ) ;
#6023 = AXIS2_PLACEMENT_3D ( 'NONE', #9218, #6879, #8327 ) ;
#6024 = ADVANCED_FACE ( 'NONE', ( #8727 ), #9365, .T. ) ;
#6025 = CARTESIAN_POINT ( 'NONE',  ( 0.000000000000000000, 0.000000000000000000, 0.000000000000000000 ) ) ;
#6026 = VERTEX_POINT ( 'NONE', #1123 ) ;
#6027 = CARTESIAN_POINT ( 'NONE',  ( -7.123219286842091158, 59.18149658568252391, 35.02766888370170051 ) ) ;
#6028 = ORIENTED_EDGE ( 'NONE', *, *, #1694, .F. ) ;
#6029 = CIRCLE ( 'NONE', #7300, 4.500000000000004441 ) ;
#6030 = PRODUCT_DEFINITION_CONTEXT ( 'detailed design', #1394, 'design' ) ;
#6031 = VERTEX_POINT ( 'NONE', #7848 ) ;
#6032 = CARTESIAN_POINT ( 'NONE',  ( -5.562309845534584518, 60.99999999999999289, 35.56426808735054834 ) ) ;
#6033 = CARTESIAN_POINT ( 'NONE',  ( 7.592786212752238627E-27, 43.00000000000019895, -24.09806918451537072 ) ) ;
#6034 = CARTESIAN_POINT ( 'NONE',  ( 4.035851918958802464, -8.834948306663564566, 39.24029717320215127 ) ) ;
#6035 = ORIENTED_EDGE ( 'NONE', *, *, #2251, .T. ) ;
#6036 = CARTESIAN_POINT ( 'NONE',  ( -2.008133409164426730, 27.99999999999992184, 31.00000000000000711 ) ) ;
#6037 = ORIENTED_EDGE ( 'NONE', *, *, #9093, .F. ) ;
#6038 = ADVANCED_FACE ( 'NONE', ( #8775 ), #7236, .F. ) ;
#6039 = CARTESIAN_POINT ( 'NONE',  ( 6.105199365910152665, -4.651526790810022405, 43.04426269254581428 ) ) ;
#6040 = DIRECTION ( 'NONE',  ( 2.168404344971006649E-16, -0.000000000000000000, 1.000000000000000000 ) ) ;
#6041 = DIRECTION ( 'NONE',  ( -1.000000000000000000, -0.000000000000000000, -0.000000000000000000 ) ) ;
#6042 = LINE ( 'NONE', #7550, #336 ) ;
#6043 = VECTOR ( 'NONE', #7853, 1000.000000000000000 ) ;
#6044 = DIRECTION ( 'NONE',  ( 0.000000000000000000, -1.000000000000000000, 0.000000000000000000 ) ) ;
#6045 = DIRECTION ( 'NONE',  ( 0.000000000000000000, 0.000000000000000000, 1.000000000000000000 ) ) ;
#6046 = EDGE_CURVE ( 'NONE', #2330, #1923, #8540, .T. ) ;
#6047 = EDGE_CURVE ( 'NONE', #9236, #156, #6491, .T. ) ;
#6048 = AXIS2_PLACEMENT_3D ( 'NONE', #6200, #1666, #9182 ) ;
#6049 = CIRCLE ( 'NONE', #871, 30.00000000000000711 ) ;
#6050 = EDGE_CURVE ( 'NONE', #982, #1104, #7936, .T. ) ;
#6051 = DIRECTION ( 'NONE',  ( 7.666467083416970531E-17, 0.7071067811865375807, 0.7071067811865574537 ) ) ;
#6052 = CARTESIAN_POINT ( 'NONE',  ( -3.999999999999999112, 0.000000000000000000, 24.67792535850613334 ) ) ;
#6053 = PRODUCT ( 'Metal Body for Mounting Threaded Chasers', 'Metal Body for Mounting Threaded Chasers', '', ( #63 ) ) ;
#6054 = EDGE_LOOP ( 'NONE', ( #7958, #6230, #8348, #718 ) ) ;
#6055 = DIRECTION ( 'NONE',  ( 0.3286710990610922090, 6.289316826390952918E-29, 0.9444444444444435316 ) ) ;
#6056 = CARTESIAN_POINT ( 'NONE',  ( 6.933488530059848109, -15.00000000000000000, 36.84292232056203886 ) ) ;
#6057 = VERTEX_POINT ( 'NONE', #4875 ) ;
#6058 = VECTOR ( 'NONE', #8899, 1000.000000000000000 ) ;
#6059 = CIRCLE ( 'NONE', #9074, 5.000000000000000000 ) ;
#6060 = ADVANCED_FACE ( 'NONE', ( #445 ), #4285, .F. ) ;
#6061 = ADVANCED_FACE ( 'NONE', ( #2586 ), #9238, .T. ) ;
#6062 = CARTESIAN_POINT ( 'NONE',  ( 0.000000000000000000, 59.99999999999999289, 0.000000000000000000 ) ) ;
#6063 = EDGE_CURVE ( 'NONE', #4609, #9521, #4239, .T. ) ;
#6064 = DIRECTION ( 'NONE',  ( -0.000000000000000000, -0.000000000000000000, 1.000000000000000000 ) ) ;
#6065 = ORIENTED_EDGE ( 'NONE', *, *, #7259, .T. ) ;
#6066 = EDGE_CURVE ( 'NONE', #4597, #6854, #9426, .T. ) ;
#6067 = AXIS2_PLACEMENT_3D ( 'NONE', #3654, #8892, #8989 ) ;
#6068 = VECTOR ( 'NONE', #5735, 1000.000000000000000 ) ;
#6069 = CARTESIAN_POINT ( 'NONE',  ( 9.737083392141938631, 0.9931181127733758052, 41.50525870069961343 ) ) ;
#6070 = AXIS2_PLACEMENT_3D ( 'NONE', #9406, #1100, #3426 ) ;
#6071=STYLED_ITEM('',(#9771),#6323);
#6072 = ORIENTED_EDGE ( 'NONE', *, *, #4496, .F. ) ;
#6073 = PLANE ( 'NONE',  #4835 ) ;
#6074 = DIRECTION ( 'NONE',  ( 0.000000000000000000, 1.000000000000000000, 0.000000000000000000 ) ) ;
#6075 = CARTESIAN_POINT ( 'NONE',  ( -5.562309845534700870, 60.99999999999999289, 28.56426808735051992 ) ) ;
#6076 = ORIENTED_EDGE ( 'NONE', *, *, #2991, .F. ) ;
#6077 = CARTESIAN_POINT ( 'NONE',  ( 4.000000000000007994, 0.000000000000000000, 24.67792535850613334 ) ) ;
#6078 = ORIENTED_EDGE ( 'NONE', *, *, #7518, .T. ) ;
#6079 = AXIS2_PLACEMENT_3D ( 'NONE', #5339, #6064, #848 ) ;
#6080 = DIRECTION ( 'NONE',  ( -0.000000000000000000, 1.000000000000000000, -0.000000000000000000 ) ) ;
#6081 = AXIS2_PLACEMENT_3D ( 'NONE', #9738, #5395, #124 ) ;
#6082 = DIRECTION ( 'NONE',  ( -0.000000000000000000, -1.000000000000000000, -0.000000000000000000 ) ) ;
#6083 = CARTESIAN_POINT ( 'NONE',  ( -6.858200383473443296, -3.989910541781668485, 42.78193147746105751 ) ) ;
#6084 = VECTOR ( 'NONE', #1119, 1000.000000000000000 ) ;
#6085 = ADVANCED_BREP_SHAPE_REPRESENTATION ( '', ( #6272, #6314 ), #2843 ) ;
#6086 = ORIENTED_EDGE ( 'NONE', *, *, #6951, .T. ) ;
#6087 = CARTESIAN_POINT ( 'NONE',  ( -8.063708916478040223, 59.93271281907998826, 32.87005020308307479 ) ) ;
#6088 = CLOSED_SHELL ( 'NONE', ( #2179, #4333, #5886, #4143, #164, #9626, #5640, #6060, #1656, #6294, #217, #9658, #9447, #8235, #3909, #2418, #793, #4321, #6357, #4176, #5415, #1271, #2439, #9524, #8912, #8215, #2497, #5033, #6464, #9579, #771, #4915, #524, #2974, #6597, #9509, #1127, #150, #3848, #2797, #8389, #770, #8969, #762, #1837, #5442, #9017, #3778, #2242, #6246, #6722, #5271, #7150, #6492 ) ) ;
#6089 = VERTEX_POINT ( 'NONE', #1906 ) ;
#6090 = PRODUCT_RELATED_PRODUCT_CATEGORY ( 'part', '', ( #8602 ) ) ;
#6091 = ORIENTED_EDGE ( 'NONE', *, *, #1672, .F. ) ;
#6092 = CARTESIAN_POINT ( 'NONE',  ( -5.942969066593652094, -10.15910374927029736, 38.55304109327786222 ) ) ;
#6093 = DIRECTION ( 'NONE',  ( 1.735493991486225972E-29, -6.508102468073347395E-30, -1.000000000000000000 ) ) ;
#6094 = CIRCLE ( 'NONE', #9569, 5.000000000000001776 ) ;
#6095 = DIRECTION ( 'NONE',  ( 0.000000000000000000, 0.000000000000000000, 1.000000000000000000 ) ) ;
#6096 = ORIENTED_EDGE ( 'NONE', *, *, #521, .T. ) ;
#6097 = DIRECTION ( 'NONE',  ( -0.9449569463147374782, 0.000000000000000000, -0.3271946967961527619 ) ) ;
#6098 = FACE_OUTER_BOUND ( 'NONE', #472, .T. ) ;
#6099 = ORIENTED_EDGE ( 'NONE', *, *, #9562, .T. ) ;
#6100 = CARTESIAN_POINT ( 'NONE',  ( 7.931830219867401333, -2.829627378531556658, 42.36468407235587819 ) ) ;
#6101 = CARTESIAN_POINT ( 'NONE',  ( 4.397412886516829822, 59.29888504437717955, -35.28275170782140435 ) ) ;
#6102 = CARTESIAN_POINT ( 'NONE',  ( 3.475261766519177176, -15.00000000000000178, 29.62668451659027014 ) ) ;
#6103 = LINE ( 'NONE', #2343, #176 ) ;
#6104 = ORIENTED_EDGE ( 'NONE', *, *, #9328, .T. ) ;
#6105 = CARTESIAN_POINT ( 'NONE',  ( -32.05305536707737701, 59.99999999999999289, -7.848671329280701769 ) ) ;
#6106 = EDGE_CURVE ( 'NONE', #3950, #77, #5617, .T. ) ;
#6107 = CARTESIAN_POINT ( 'NONE',  ( -8.216777476527294510, 44.00000000000019895, -23.61111111111111427 ) ) ;
#6108 = ORIENTED_EDGE ( 'NONE', *, *, #8735, .T. ) ;
#6109 = CARTESIAN_POINT ( 'NONE',  ( -33.06426808735054124, 60.99999999999999289, -1.062309845534581632 ) ) ;
#6110 = CARTESIAN_POINT ( 'NONE',  ( 5.540660272217056814, -15.00000000000031619, 36.79964862145148174 ) ) ;
#6111 = ORIENTED_EDGE ( 'NONE', *, *, #4973, .F. ) ;
#6112 = CARTESIAN_POINT ( 'NONE',  ( 9.417027056075828427E-27, 44.50000000000019185, -25.00000000000000000 ) ) ;
#6113 =( REPRESENTATION_RELATIONSHIP ('NONE','NONE', #5841, #551 ) REPRESENTATION_RELATIONSHIP_WITH_TRANSFORMATION ( #11 )SHAPE_REPRESENTATION_RELATIONSHIP( ) );
#6114 = CARTESIAN_POINT ( 'NONE',  ( 0.000000000000000000, -0.7216878364870317197, -1.250000000000000000 ) ) ;
#6115 = VERTEX_POINT ( 'NONE', #8579 ) ;
#6116 = CARTESIAN_POINT ( 'NONE',  ( 12.83676879653350866, -0.6422030776960447884, 36.82710757287565428 ) ) ;
#6117 = ORIENTED_EDGE ( 'NONE', *, *, #1841, .T. ) ;
#6118 = CARTESIAN_POINT ( 'NONE',  ( 32.59762842694625817, 60.99999999999999289, -5.137569555611371186 ) ) ;
#6119 = EDGE_CURVE ( 'NONE', #6057, #1263, #2752, .T. ) ;
#6120 = PLANE ( 'NONE',  #2498 ) ;
#6121 = DIRECTION ( 'NONE',  ( 1.735493991486227934E-29, 0.000000000000000000, -1.000000000000000000 ) ) ;
#6122 = EDGE_CURVE ( 'NONE', #2716, #7071, #8276, .T. ) ;
#6123 = ORIENTED_EDGE ( 'NONE', *, *, #9244, .F. ) ;
#6124 = CARTESIAN_POINT ( 'NONE',  ( 30.18708036726505028, 60.99999999999999289, 16.70299909897265778 ) ) ;
#6125 = EDGE_CURVE ( 'NONE', #6002, #1252, #5565, .T. ) ;
#6126 = EDGE_LOOP ( 'NONE', ( #1329, #5794, #7472, #5528 ) ) ;
#6127 = DIRECTION ( 'NONE',  ( 0.000000000000000000, 1.000000000000000000, 0.000000000000000000 ) ) ;
#6128 = DIRECTION ( 'NONE',  ( 0.000000000000000000, -0.000000000000000000, 1.000000000000000000 ) ) ;
#6129 = CARTESIAN_POINT ( 'NONE',  ( -6.123066174590870325, -4.617945597878252428, 43.03242323456579754 ) ) ;
#6130 = ORIENTED_EDGE ( 'NONE', *, *, #2372, .T. ) ;
#6131 = CARTESIAN_POINT ( 'NONE',  ( -7.989536001449261349, 59.73029374780620060, 33.69619452719667407 ) ) ;
#6132 = VERTEX_POINT ( 'NONE', #7082 ) ;
#6133 = CIRCLE ( 'NONE', #1875, 25.00000000000000000 ) ;
#6134 = ORIENTED_EDGE ( 'NONE', *, *, #2384, .F. ) ;
#6135 = DIRECTION ( 'NONE',  ( -1.820952055660014662E-28, -1.000000000000000000, -7.038118388768679669E-30 ) ) ;
#6136 = DIRECTION ( 'NONE',  ( -0.000000000000000000, 1.000000000000000000, -0.000000000000000000 ) ) ;
#6137 = VECTOR ( 'NONE', #5345, 1000.000000000000000 ) ;
#6138 = CIRCLE ( 'NONE', #1886, 4.999999999999997335 ) ;
#6139 = EDGE_LOOP ( 'NONE', ( #6846, #8357 ) ) ;
#6140 = CYLINDRICAL_SURFACE ( 'NONE', #8366, 4.500000000000004441 ) ;
#6141 = CARTESIAN_POINT ( 'NONE',  ( 31.00000000000000711, -15.00000000000000000, 6.000000000000000000 ) ) ;
#6142 = ORIENTED_EDGE ( 'NONE', *, *, #7743, .T. ) ;
#6143 = LINE ( 'NONE', #9176, #5071 ) ;
#6144 = CARTESIAN_POINT ( 'NONE',  ( 3.147661243663450126, 59.92470504718686897, -33.73534932023821398 ) ) ;
#6145 = CARTESIAN_POINT ( 'NONE',  ( 4.653657836759942730E-15, 54.99999999999999289, -38.00000000000000711 ) ) ;
#6146 = CARTESIAN_POINT ( 'NONE',  ( -8.237197373723139648, -15.00000000000000000, 27.80554943579302929 ) ) ;
#6147 = CARTESIAN_POINT ( 'NONE',  ( 0.000000000000000000, 59.99999999999999289, 0.000000000000000000 ) ) ;
#6148 = DIRECTION ( 'NONE',  ( -1.000000000000000000, 0.000000000000000000, 0.000000000000000000 ) ) ;
#6149 = VERTEX_POINT ( 'NONE', #334 ) ;
#6150 = CIRCLE ( 'NONE', #3309, 1.500000000000001332 ) ;
#6151 = CARTESIAN_POINT ( 'NONE',  ( 8.677469957431129860E-27, 40.00000000000014921, -25.00000000000000000 ) ) ;
#6152 = EDGE_CURVE ( 'NONE', #6918, #5598, #3338, .T. ) ;
#6153 = AXIS2_PLACEMENT_3D ( 'NONE', #8684, #4094, #1908 ) ;
#6154 = ORIENTED_EDGE ( 'NONE', *, *, #3650, .F. ) ;
#6155 = CARTESIAN_POINT ( 'NONE',  ( -8.216777476527294510, 40.00000000000014921, -23.61111111111111427 ) ) ;
#6156 = VERTEX_POINT ( 'NONE', #5069 ) ;
#6157 = FACE_OUTER_BOUND ( 'NONE', #7560, .T. ) ;
#6158 = CARTESIAN_POINT ( 'NONE',  ( 37.01190402608325059, 62.00000000000000711, 3.384896555618068348 ) ) ;
#6159 = ORIENTED_EDGE ( 'NONE', *, *, #6951, .F. ) ;
#6160 = DIRECTION ( 'NONE',  ( 0.000000000000000000, 0.000000000000000000, 1.000000000000000000 ) ) ;
#6161 = CARTESIAN_POINT ( 'NONE',  ( -6.000000000000005329, 27.42469319230600533, -31.00000000000000711 ) ) ;
#6162 = EDGE_LOOP ( 'NONE', ( #6863, #9405, #5196, #2465, #3016 ) ) ;
#6163 = CARTESIAN_POINT ( 'NONE',  ( 6.290056143031378610, -4.520955051545493042, 38.59677555533873772 ) ) ;
#6164 = CARTESIAN_POINT ( 'NONE',  ( -33.06426808735054124, 61.99999999999999289, -10.06230984553459251 ) ) ;
#6165 = EDGE_LOOP ( 'NONE', ( #8717, #8003, #7613, #318 ) ) ;
#6166 = DIRECTION ( 'NONE',  ( -0.000000000000000000, 1.000000000000000000, -0.000000000000000000 ) ) ;
#6167 = ORIENTED_EDGE ( 'NONE', *, *, #9384, .T. ) ;
#6168 = DIRECTION ( 'NONE',  ( 0.000000000000000000, -0.000000000000000000, 1.000000000000000000 ) ) ;
#6169 = AXIS2_PLACEMENT_3D ( 'NONE', #1459, #1413, #6736 ) ;
#6170 = ORIENTED_EDGE ( 'NONE', *, *, #6662, .F. ) ;
#6171 = CARTESIAN_POINT ( 'NONE',  ( 25.23917843705063646, 29.66524321760768501, -4.665243217607707216 ) ) ;
#6172 = LINE ( 'NONE', #7717, #5566 ) ;
#6173 = EDGE_CURVE ( 'NONE', #8145, #1128, #8129, .T. ) ;
#6174 = CIRCLE ( 'NONE', #7448, 2.499999999999998668 ) ;
#6175 = EDGE_CURVE ( 'NONE', #5322, #7811, #4498, .T. ) ;
#6176 = EDGE_CURVE ( 'NONE', #3412, #8756, #8870, .T. ) ;
#6177 = ORIENTED_EDGE ( 'NONE', *, *, #3476, .T. ) ;
#6178 = CARTESIAN_POINT ( 'NONE',  ( -10.79742499427308289, 54.99999999999999289, 31.18357922838633201 ) ) ;
#6179 = ORIENTED_EDGE ( 'NONE', *, *, #7007, .T. ) ;
#6180 = ORIENTED_EDGE ( 'NONE', *, *, #8964, .T. ) ;
#6181 = ORIENTED_EDGE ( 'NONE', *, *, #5013, .F. ) ;
#6182 = CARTESIAN_POINT ( 'NONE',  ( -4.469925451758544277, -5.674451673807808127, 43.49573866965157976 ) ) ;
#6183 = CIRCLE ( 'NONE', #3190, 1.499999999999999556 ) ;
#6184 = DIRECTION ( 'NONE',  ( -0.9449569463147374782, 0.000000000000000000, -0.3271946967961527619 ) ) ;
#6185 = CARTESIAN_POINT ( 'NONE',  ( 0.000000000000000000, 30.00000000000000000, 0.000000000000000000 ) ) ;
#6186 = EDGE_CURVE ( 'NONE', #1776, #2818, #8920, .T. ) ;
#6187 = ADVANCED_FACE ( 'NONE', ( #8080 ), #5212, .F. ) ;
#6188 = AXIS2_PLACEMENT_3D ( 'NONE', #2724, #5698, #3432 ) ;
#6189 = ORIENTED_EDGE ( 'NONE', *, *, #7940, .F. ) ;
#6190 = CARTESIAN_POINT ( 'NONE',  ( -15.97678174684350871, 60.99999999999999289, 28.87459861216650836 ) ) ;
#6191 = CYLINDRICAL_SURFACE ( 'NONE', #4887, 40.00000000000000711 ) ;
#6192 = VECTOR ( 'NONE', #5278, 1000.000000000000000 ) ;
#6193 = ORIENTED_EDGE ( 'NONE', *, *, #1407, .T. ) ;
#6194 = CARTESIAN_POINT ( 'NONE',  ( 0.000000000000000000, 19.99999999999982236, 0.000000000000000000 ) ) ;
#6195 = CARTESIAN_POINT ( 'NONE',  ( 5.562309845551833831, 59.00253480853272947, -35.56426808735054834 ) ) ;
#6196 = PLANE ( 'NONE',  #2033 ) ;
#6197 = CARTESIAN_POINT ( 'NONE',  ( 6.168569856766713322, 16.58737218350495723, 38.51007260663249099 ) ) ;
#6198 = DIRECTION ( 'NONE',  ( 0.000000000000000000, 0.000000000000000000, 1.000000000000000000 ) ) ;
#6199 = EDGE_LOOP ( 'NONE', ( #5736, #3541, #3727, #1873 ) ) ;
#6200 = CARTESIAN_POINT ( 'NONE',  ( 1.555535097482682654E-26, 78.08723716182652197, -25.00000000000000000 ) ) ;
#6201 = CARTESIAN_POINT ( 'NONE',  ( 33.06426808735054124, 60.99999999999999289, 5.562309845534586294 ) ) ;
#6202 = VERTEX_POINT ( 'NONE', #5117 ) ;
#6203 = DIRECTION ( 'NONE',  ( -1.000000000000000000, -0.000000000000000000, -0.000000000000000000 ) ) ;
#6204 = LINE ( 'NONE', #7856, #4055 ) ;
#6205 = EDGE_CURVE ( 'NONE', #7344, #9409, #8918, .T. ) ;
#6206 = ORIENTED_EDGE ( 'NONE', *, *, #7147, .F. ) ;
#6207 = DIRECTION ( 'NONE',  ( -0.000000000000000000, -1.000000000000000000, -0.000000000000000000 ) ) ;
#6208 = CIRCLE ( 'NONE', #8581, 26.00000000000002132 ) ;
#6209 = LINE ( 'NONE', #6114, #3558 ) ;
#6210 = ORIENTED_EDGE ( 'NONE', *, *, #2329, .T. ) ;
#6211 = CARTESIAN_POINT ( 'NONE',  ( -8.216777476527294510, 60.00000000000029843, -23.61111111111107519 ) ) ;
#6212 = DIRECTION ( 'NONE',  ( 1.000000000000000000, 0.000000000000000000, -2.168404344971006649E-16 ) ) ;
#6213 = ORIENTED_EDGE ( 'NONE', *, *, #6175, .F. ) ;
#6214 = VECTOR ( 'NONE', #8539, 1000.000000000000000 ) ;
#6215 = CARTESIAN_POINT ( 'NONE',  ( 0.000000000000000000, 59.99999999999999289, 0.000000000000000000 ) ) ;
#6216 = ORIENTED_EDGE ( 'NONE', *, *, #9427, .F. ) ;
#6217 = DIRECTION ( 'NONE',  ( 0.000000000000000000, 0.000000000000000000, 1.000000000000000000 ) ) ;
#6218 = VERTEX_POINT ( 'NONE', #7338 ) ;
#6219 = PRODUCT_DEFINITION_SHAPE ( 'NONE', 'NONE',  #1863 ) ;
#6220 = DIRECTION ( 'NONE',  ( 0.000000000000000000, 1.000000000000000000, 0.000000000000000000 ) ) ;
#6221 = CARTESIAN_POINT ( 'NONE',  ( -6.620899530561116464, -4.206347570868084418, 42.86624096190644906 ) ) ;
#6222 = AXIS2_PLACEMENT_3D ( 'NONE', #1391, #2774, #5793 ) ;
#6223 = VECTOR ( 'NONE', #4189, 1000.000000000000000 ) ;
#6224 = EDGE_CURVE ( 'NONE', #6218, #300, #3585, .T. ) ;
#6225 = ORIENTED_EDGE ( 'NONE', *, *, #9297, .F. ) ;
#6226 = CARTESIAN_POINT ( 'NONE',  ( 29.00000000000000355, 30.00000000000000000, 4.000000000000000000 ) ) ;
#6227 = CIRCLE ( 'NONE', #3394, 28.99999999999995026 ) ;
#6228 = ORIENTED_EDGE ( 'NONE', *, *, #8364, .F. ) ;
#6229 = DIRECTION ( 'NONE',  ( 0.000000000000000000, 0.000000000000000000, -1.000000000000000000 ) ) ;
#6230 = ORIENTED_EDGE ( 'NONE', *, *, #1012, .T. ) ;
#6231 = VECTOR ( 'NONE', #2874, 1000.000000000000000 ) ;
#6232 = EDGE_CURVE ( 'NONE', #1238, #8006, #721, .T. ) ;
#6233 = EDGE_LOOP ( 'NONE', ( #123, #1541, #3820, #4227 ) ) ;
#6234 = VECTOR ( 'NONE', #6635, 1000.000000000000000 ) ;
#6235 =( GEOMETRIC_REPRESENTATION_CONTEXT ( 3 ) GLOBAL_UNCERTAINTY_ASSIGNED_CONTEXT ( ( #814 ) ) GLOBAL_UNIT_ASSIGNED_CONTEXT ( ( #3122, #5414, #6921 ) ) REPRESENTATION_CONTEXT ( 'NONE', 'WORKASPACE' ) );
#6236 = CARTESIAN_POINT ( 'NONE',  ( -9.920757921939857837, 1.831472460275451519, 37.87927513041881866 ) ) ;
#6237 = EDGE_CURVE ( 'NONE', #6854, #2236, #2882, .T. ) ;
#6238 = CARTESIAN_POINT ( 'NONE',  ( 0.01843853345419280837, 13.29483547765106799, 43.99999130734108377 ) ) ;
#6239 = PLANE ( 'NONE',  #9039 ) ;
#6240 = VECTOR ( 'NONE', #2817, 1000.000000000000000 ) ;
#6241 = ORIENTED_EDGE ( 'NONE', *, *, #1725, .F. ) ;
#6242 = CARTESIAN_POINT ( 'NONE',  ( 18.58791755254457811, 59.99999999999999289, 23.54759692749571443 ) ) ;
#6243 = EDGE_LOOP ( 'NONE', ( #9545, #8355, #7311, #8471 ) ) ;
#6244 = DIRECTION ( 'NONE',  ( -0.000000000000000000, -1.000000000000000000, -0.000000000000000000 ) ) ;
#6245 = CARTESIAN_POINT ( 'NONE',  ( -4.999999999999813483, 19.99999999999990408, -20.00000000000019185 ) ) ;
#6246 = ADVANCED_FACE ( 'NONE', ( #6539 ), #4477, .F. ) ;
#6247 = AXIS2_PLACEMENT_3D ( 'NONE', #7360, #8744, #3413 ) ;
#6248 = CARTESIAN_POINT ( 'NONE',  ( 0.000000000000000000, 59.99999999999999289, 0.000000000000000000 ) ) ;
#6249 = EDGE_CURVE ( 'NONE', #8321, #9687, #9540, .T. ) ;
#6250 = LINE ( 'NONE', #9275, #4433 ) ;
#6251 = EDGE_CURVE ( 'NONE', #6987, #3873, #5986, .T. ) ;
#6252 = CARTESIAN_POINT ( 'NONE',  ( -33.06426808735054124, 69.99999999999998579, -3.062309845534580077 ) ) ;
#6253 = VECTOR ( 'NONE', #5714, 1000.000000000000114 ) ;
#6254 = DIRECTION ( 'NONE',  ( 0.000000000000000000, -1.000000000000000000, 0.000000000000000000 ) ) ;
#6255 = ORIENTED_EDGE ( 'NONE', *, *, #3414, .F. ) ;
#6256 = CARTESIAN_POINT ( 'NONE',  ( 6.235648121649441045, 61.81426382726520075, -37.52627707316309369 ) ) ;
#6257 = DIRECTION ( 'NONE',  ( 0.000000000000000000, 0.000000000000000000, 1.000000000000000000 ) ) ;
#6258 = ORIENTED_EDGE ( 'NONE', *, *, #6843, .T. ) ;
#6259 = PLANE ( 'NONE',  #7454 ) ;
#6260 = CARTESIAN_POINT ( 'NONE',  ( -37.54740336257584232, 61.81808349686849624, -6.037872445562960877 ) ) ;
#6261 = EDGE_CURVE ( 'NONE', #1692, #7344, #6630, .T. ) ;
#6262 = CARTESIAN_POINT ( 'NONE',  ( 0.6466180781814862000, -6.706436388010658334, 44.00065907709070245 ) ) ;
#6263 = CONTEXT_DEPENDENT_SHAPE_REPRESENTATION ( #8467, #7648 ) ;
#6264 = FACE_OUTER_BOUND ( 'NONE', #1435, .T. ) ;
#6265 = ORIENTED_EDGE ( 'NONE', *, *, #3689, .T. ) ;
#6266 = CARTESIAN_POINT ( 'NONE',  ( -35.88888888888889284, 54.99999999999999289, 12.48950176432140857 ) ) ;
#6267 = ORIENTED_EDGE ( 'NONE', *, *, #2231, .F. ) ;
#6268 = CARTESIAN_POINT ( 'NONE',  ( 1.148778693228098442E-26, 57.50000000000029843, -25.00000000000000000 ) ) ;
#6269 = VERTEX_POINT ( 'NONE', #6728 ) ;
#6270 = DIRECTION ( 'NONE',  ( 0.000000000000000000, 0.000000000000000000, 1.000000000000000000 ) ) ;
#6271 = CARTESIAN_POINT ( 'NONE',  ( -36.86535760663189620, 61.99999999999999289, -3.153634179030289530 ) ) ;
#6272 = MANIFOLD_SOLID_BREP ( 'Chamfer4', #120 ) ;
#6273 = ORIENTED_EDGE ( 'NONE', *, *, #5945, .T. ) ;
#6274 = DIRECTION ( 'NONE',  ( -0.9860132971832693549, -1.788557213313974126E-28, 0.1666666666666657970 ) ) ;
#6275 = ORIENTED_EDGE ( 'NONE', *, *, #3332, .T. ) ;
#6276 = LINE ( 'NONE', #7169, #6388 ) ;
#6277 = ORIENTED_EDGE ( 'NONE', *, *, #9704, .F. ) ;
#6278 = ORIENTED_EDGE ( 'NONE', *, *, #8114, .F. ) ;
#6279 = CARTESIAN_POINT ( 'NONE',  ( -13.27241307482885802, 4.308278809869828585, 36.67213216020381594 ) ) ;
#6280 = DIRECTION ( 'NONE',  ( -0.000000000000000000, 1.000000000000000000, -0.000000000000000000 ) ) ;
#6281 = DIRECTION ( 'NONE',  ( -0.000000000000000000, 1.000000000000000000, -0.000000000000000000 ) ) ;
#6282 = ORIENTED_EDGE ( 'NONE', *, *, #9268, .F. ) ;
#6283 = DIRECTION ( 'NONE',  ( 0.000000000000000000, 0.000000000000000000, -1.000000000000000000 ) ) ;
#6284 = ORIENTED_EDGE ( 'NONE', *, *, #5301, .F. ) ;
#6285 = CARTESIAN_POINT ( 'NONE',  ( -12.16083066526040213, 78.08723716182652197, -34.94444444444459918 ) ) ;
#6286 = DIRECTION ( 'NONE',  ( -0.000000000000000000, -1.000000000000000000, -0.000000000000000000 ) ) ;
#6287 = DIRECTION ( 'NONE',  ( 0.000000000000000000, 0.000000000000000000, 1.000000000000000000 ) ) ;
#6288 = CARTESIAN_POINT ( 'NONE',  ( 0.000000000000000000, 39.99999999999999289, 0.000000000000000000 ) ) ;
#6289 = DIRECTION ( 'NONE',  ( -1.000000000000000000, 0.000000000000000000, 0.000000000000000000 ) ) ;
#6290 = DIRECTION ( 'NONE',  ( 0.000000000000000000, 1.000000000000000000, 0.000000000000000000 ) ) ;
#6291 = CIRCLE ( 'NONE', #8189, 39.00000000000002132 ) ;
#6292 = EDGE_CURVE ( 'NONE', #9059, #8698, #8221, .T. ) ;
#6293 = EDGE_CURVE ( 'NONE', #1923, #5073, #5132, .T. ) ;
#6294 = ADVANCED_FACE ( 'NONE', ( #4718 ), #918, .F. ) ;
#6295 = ORIENTED_EDGE ( 'NONE', *, *, #7649, .T. ) ;
#6296 = DIRECTION ( 'NONE',  ( -0.001843853345419366619, -0.9999983001009754568, 0.000000000000000000 ) ) ;
#6297 = APPLICATION_CONTEXT ( 'automotive_design' ) ;
#6298 = AXIS2_PLACEMENT_3D ( 'NONE', #5217, #624, #3783 ) ;
#6299 = ORIENTED_EDGE ( 'NONE', *, *, #2424, .F. ) ;
#6300 = LINE ( 'NONE', #3193, #388 ) ;
#6301 = EDGE_LOOP ( 'NONE', ( #8651, #4322, #9671, #2472 ) ) ;
#6302 = DIRECTION ( 'NONE',  ( 0.000000000000000000, -1.000000000000000000, 0.000000000000000000 ) ) ;
#6303 = CARTESIAN_POINT ( 'NONE',  ( 10.00000000000001599, 3.294852476641296768, 184.6745183374407020 ) ) ;
#6304 = ORIENTED_EDGE ( 'NONE', *, *, #9461, .F. ) ;
#6305 = CARTESIAN_POINT ( 'NONE',  ( -9.669395431759557624, 5.928981332583603603, 41.54124299433283340 ) ) ;
#6306 = CARTESIAN_POINT ( 'NONE',  ( 0.000000000000000000, 58.99999999999999289, 0.000000000000000000 ) ) ;
#6307 = AXIS2_PLACEMENT_3D ( 'NONE', #3439, #1948, #2736 ) ;
#6308 = CARTESIAN_POINT ( 'NONE',  ( 4.898587196589413815E-15, 58.99999999999999289, 40.00000000000000711 ) ) ;
#6309 = EDGE_CURVE ( 'NONE', #1104, #9236, #2282, .T. ) ;
#6310 = FACE_OUTER_BOUND ( 'NONE', #6829, .T. ) ;
#6311 = EDGE_CURVE ( 'NONE', #285, #8477, #888, .T. ) ;
#6312 = EDGE_LOOP ( 'NONE', ( #1893, #3368, #836, #3170, #4410 ) ) ;
#6313 = CARTESIAN_POINT ( 'NONE',  ( 0.000000000000000000, 59.99999999999999289, 0.000000000000000000 ) ) ;
#6314 = AXIS2_PLACEMENT_3D ( 'NONE', #9654, #2830, #5168 ) ;
#6315 = ORIENTED_EDGE ( 'NONE', *, *, #988, .F. ) ;
#6316 = DIRECTION ( 'NONE',  ( -0.000000000000000000, 1.000000000000000000, -0.000000000000000000 ) ) ;
#6317 = ORIENTED_EDGE ( 'NONE', *, *, #9704, .T. ) ;
#6318 = DIRECTION ( 'NONE',  ( -0.000000000000000000, 1.000000000000000000, -0.000000000000000000 ) ) ;
#6319 = ORIENTED_EDGE ( 'NONE', *, *, #9328, .F. ) ;
#6320 = DIRECTION ( 'NONE',  ( 0.000000000000000000, 0.000000000000000000, -1.000000000000000000 ) ) ;
#6321 = DIRECTION ( 'NONE',  ( 0.1666666666666662411, 3.900547397768555245E-29, 0.9860132971832694659 ) ) ;
#6322 = VECTOR ( 'NONE', #4684, 1000.000000000000000 ) ;
#6323 = MANIFOLD_SOLID_BREP ( 'Chamfer5', #3571 ) ;
#6324 = VERTEX_POINT ( 'NONE', #6238 ) ;
#6325 = DIRECTION ( 'NONE',  ( -0.000000000000000000, 1.000000000000000000, -0.000000000000000000 ) ) ;
#6326 = ORIENTED_EDGE ( 'NONE', *, *, #3270, .F. ) ;
#6327 = DIRECTION ( 'NONE',  ( -1.820952055660014662E-28, -1.000000000000000000, -7.038118388768679669E-30 ) ) ;
#6328 = EDGE_LOOP ( 'NONE', ( #1535, #9625, #8660, #3577 ) ) ;
#6329 = ORIENTED_EDGE ( 'NONE', *, *, #7081, .T. ) ;
#6330 = CARTESIAN_POINT ( 'NONE',  ( -9.866411883523234394, 4.956617588930513740, 41.43648181959947152 ) ) ;
#6331 = B_SPLINE_CURVE_WITH_KNOTS ( 'NONE', 3,
 ( #7343, #585, #4427, #7438 ),
 .UNSPECIFIED., .F., .F.,
 ( 4, 4 ),
 ( 0.000000000000000000, 0.001643226871903045875 ),
 .UNSPECIFIED. ) ;
#6332 = EDGE_CURVE ( 'NONE', #1017, #3027, #4036, .T. ) ;
#6333 = FACE_OUTER_BOUND ( 'NONE', #6233, .T. ) ;
#6334 = VECTOR ( 'NONE', #4947, 1000.000000000000114 ) ;
#6335 = FACE_OUTER_BOUND ( 'NONE', #4896, .T. ) ;
#6336 = ORIENTED_EDGE ( 'NONE', *, *, #6425, .F. ) ;
#6337 = DIRECTION ( 'NONE',  ( 0.000000000000000000, 1.000000000000000000, 0.000000000000000000 ) ) ;
#6338 = ORIENTED_EDGE ( 'NONE', *, *, #6125, .F. ) ;
#6339 = CARTESIAN_POINT ( 'NONE',  ( -5.562309845534701758, 60.99999999999999289, 37.56426808735052703 ) ) ;
#6340 = AXIS2_PLACEMENT_3D ( 'NONE', #9730, #4549, #743 ) ;
#6341 = CARTESIAN_POINT ( 'NONE',  ( 9.860761315262647568E-27, 49.00000000000032685, -25.00000000000000000 ) ) ;
#6342 = DIRECTION ( 'NONE',  ( 0.000000000000000000, 1.000000000000000000, 0.000000000000000000 ) ) ;
#6343 = DIRECTION ( 'NONE',  ( -1.735493991486225972E-29, 6.508102468073347395E-30, 1.000000000000000000 ) ) ;
#6344 = CARTESIAN_POINT ( 'NONE',  ( 5.562309845534588959, 69.99999999999998579, -30.56426808735054479 ) ) ;
#6345 = CARTESIAN_POINT ( 'NONE',  ( 28.34870838944214100, 59.99999999999999289, 9.815840903884559765 ) ) ;
#6346 = CIRCLE ( 'NONE', #3674, 3.000000000000002665 ) ;
#6347 = AXIS2_PLACEMENT_3D ( 'NONE', #7041, #5487, #4789 ) ;
#6348 = ADVANCED_FACE ( 'NONE', ( #5464 ), #2129, .T. ) ;
#6349 = LINE ( 'NONE', #9366, #2346 ) ;
#6350 = VERTEX_POINT ( 'NONE', #3776 ) ;
#6351 = DIRECTION ( 'NONE',  ( -1.735493991486225972E-29, 6.508102468073347395E-30, 1.000000000000000000 ) ) ;
#6352 = VERTEX_POINT ( 'NONE', #3883 ) ;
#6353 = CARTESIAN_POINT ( 'NONE',  ( 33.06426808735054124, 49.99999999999999289, 5.562309845534586294 ) ) ;
#6354 = DIRECTION ( 'NONE',  ( 0.000000000000000000, 0.000000000000000000, 1.000000000000000000 ) ) ;
#6355 = VERTEX_POINT ( 'NONE', #6773 ) ;
#6356 = DIRECTION ( 'NONE',  ( -0.000000000000000000, -1.000000000000000000, -0.000000000000000000 ) ) ;
#6357 = ADVANCED_FACE ( 'NONE', ( #30 ), #3827, .F. ) ;
#6358 = DIRECTION ( 'NONE',  ( 1.000000000000000000, 0.000000000000000000, -0.000000000000000000 ) ) ;
#6359 = LINE ( 'NONE', #2603, #892 ) ;
#6360 = DIRECTION ( 'NONE',  ( 1.735493991486226532E-29, 0.000000000000000000, -1.000000000000000000 ) ) ;
#6361 = DIRECTION ( 'NONE',  ( -0.6195972517514877209, 0.000000000000000000, -0.7849198975831889191 ) ) ;
#6362 = VERTEX_POINT ( 'NONE', #2333 ) ;
#6363 = DIRECTION ( 'NONE',  ( -0.9588120495101037921, 0.000000000000000000, 0.2840412887490734173 ) ) ;
#6364 = CARTESIAN_POINT ( 'NONE',  ( 3.796404955196288922E-15, 27.99999999999992184, 31.00000000000000711 ) ) ;
#6365 = ORIENTED_EDGE ( 'NONE', *, *, #5284, .T. ) ;
#6366 = EDGE_CURVE ( 'NONE', #7266, #2358, #2921, .T. ) ;
#6367 = ADVANCED_FACE ( 'NONE', ( #4629 ), #9167, .T. ) ;
#6368 = CIRCLE ( 'NONE', #8431, 26.00000000000000355 ) ;
#6369 = PLANE ( 'NONE',  #828 ) ;
#6370 = LINE ( 'NONE', #416, #261 ) ;
#6371 = AXIS2_PLACEMENT_3D ( 'NONE', #4984, #549, #8692 ) ;
#6372 = AXIS2_PLACEMENT_3D ( 'NONE', #5032, #8002, #8146 ) ;
#6373 = PLANE ( 'NONE',  #3619 ) ;
#6374 = EDGE_LOOP ( 'NONE', ( #3326, #114, #1620, #364 ) ) ;
#6375 = CARTESIAN_POINT ( 'NONE',  ( 0.000000000000000000, 58.99999999999999289, 0.000000000000000000 ) ) ;
#6376 = EDGE_LOOP ( 'NONE', ( #2014, #1815, #1559, #856 ) ) ;
#6377 = CYLINDRICAL_SURFACE ( 'NONE', #5911, 38.00000000000000711 ) ;
#6378 = ORIENTED_EDGE ( 'NONE', *, *, #2249, .F. ) ;
#6379 = ORIENTED_EDGE ( 'NONE', *, *, #6477, .F. ) ;
#6380 = CARTESIAN_POINT ( 'NONE',  ( -9.350470702154407121, 6.934942045775910557, 38.01926452046366478 ) ) ;
#6381 = AXIS2_PLACEMENT_3D ( 'NONE', #8046, #2894, #7207 ) ;
#6382 = CARTESIAN_POINT ( 'NONE',  ( 0.000000000000000000, 30.00000000000000000, 0.000000000000000000 ) ) ;
#6383 = AXIS2_PLACEMENT_3D ( 'NONE', #4042, #101, #8487 ) ;
#6384 = CARTESIAN_POINT ( 'NONE',  ( -8.216777476527294510, 43.00000000000019895, -23.61111111111111427 ) ) ;
#6385 = VECTOR ( 'NONE', #4846, 1000.000000000000000 ) ;
#6386 = ORIENTED_EDGE ( 'NONE', *, *, #2862, .T. ) ;
#6387 = CYLINDRICAL_SURFACE ( 'NONE', #3952, 3.799999999999999378 ) ;
#6388 = VECTOR ( 'NONE', #1790, 1000.000000000000000 ) ;
#6389 = AXIS2_PLACEMENT_3D ( 'NONE', #869, #6877, #2380 ) ;
#6390 = ORIENTED_EDGE ( 'NONE', *, *, #5695, .F. ) ;
#6391 = PLANE ( 'NONE',  #1604 ) ;
#6392 = CARTESIAN_POINT ( 'NONE',  ( 0.000000000000000000, 30.99999999999998579, 0.000000000000000000 ) ) ;
#6393 = CYLINDRICAL_SURFACE ( 'NONE', #1103, 27.00000000000000355 ) ;
#6394 = CARTESIAN_POINT ( 'NONE',  ( 33.06426808735054124, 69.99999999999998579, 5.562309845534586294 ) ) ;
#6395 = PLANE ( 'NONE',  #1420 ) ;
#6396 = DIRECTION ( 'NONE',  ( 1.000000000000000000, 0.000000000000000000, 0.000000000000000000 ) ) ;
#6397 = CIRCLE ( 'NONE', #5144, 30.00000000000000711 ) ;
#6398 = VECTOR ( 'NONE', #6710, 1000.000000000000341 ) ;
#6399 = DIRECTION ( 'NONE',  ( -0.9860132971832694659, -1.788557213313974350E-28, 0.1666666666666658247 ) ) ;
#6400 = VECTOR ( 'NONE', #897, 1000.000000000000000 ) ;
#6401 = ORIENTED_EDGE ( 'NONE', *, *, #5166, .F. ) ;
#6402 = DIRECTION ( 'NONE',  ( 0.9449569463147374782, 0.000000000000000000, 0.3271946967961528174 ) ) ;
#6403 = CARTESIAN_POINT ( 'NONE',  ( 6.622760353406874856, 10.81530383135506135, 42.86969992518040584 ) ) ;
#6404 = EDGE_LOOP ( 'NONE', ( #5331, #7658, #4289, #6513 ) ) ;
#6405 = CARTESIAN_POINT ( 'NONE',  ( 0.000000000000000000, 19.99999999999982236, 0.000000000000000000 ) ) ;
#6406 = VERTEX_POINT ( 'NONE', #7173 ) ;
#6407 = DIRECTION ( 'NONE',  ( 0.000000000000000000, 0.000000000000000000, 1.000000000000000000 ) ) ;
#6408 = DIRECTION ( 'NONE',  ( 0.000000000000000000, 0.000000000000000000, -1.000000000000000000 ) ) ;
#6409 = CIRCLE ( 'NONE', #9422, 2.500000000000002220 ) ;
#6410 = DIRECTION ( 'NONE',  ( 0.000000000000000000, 0.000000000000000000, 1.000000000000000000 ) ) ;
#6411 = DIRECTION ( 'NONE',  ( -1.820952055660014662E-28, -1.000000000000000000, -7.038118388768679669E-30 ) ) ;
#6412 = ORIENTED_EDGE ( 'NONE', *, *, #6485, .T. ) ;
#6413 = CARTESIAN_POINT ( 'NONE',  ( 0.000000000000000000, 59.99999999999999289, 0.000000000000000000 ) ) ;
#6414 = CARTESIAN_POINT ( 'NONE',  ( -10.60768798165303473, -14.99999999999749356, 37.26924479348801356 ) ) ;
#6415 = ORIENTED_EDGE ( 'NONE', *, *, #2987, .F. ) ;
#6416 = LINE ( 'NONE', #4760, #5404 ) ;
#6417 = PLANE ( 'NONE',  #5767 ) ;
#6418 = CARTESIAN_POINT ( 'NONE',  ( 0.4611600587751271130, 18.29391864775294962, 38.99971782587474678 ) ) ;
#6419 = ADVANCED_FACE ( 'NONE', ( #1889 ), #433, .F. ) ;
#6420 = EDGE_CURVE ( 'NONE', #1992, #3235, #1989, .T. ) ;
#6421 = EDGE_CURVE ( 'NONE', #6767, #3486, #1200, .T. ) ;
#6422 = CARTESIAN_POINT ( 'NONE',  ( 4.898587196589413815E-15, 30.99999999999998579, 40.00000000000000711 ) ) ;
#6423 = VERTEX_POINT ( 'NONE', #375 ) ;
#6424 = LINE ( 'NONE', #9347, #1668 ) ;
#6425 = EDGE_CURVE ( 'NONE', #5052, #7534, #7880, .T. ) ;
#6426 = ORIENTED_EDGE ( 'NONE', *, *, #7038, .T. ) ;
#6427 = DIRECTION ( 'NONE',  ( -0.000000000000000000, -1.000000000000000000, -0.000000000000000000 ) ) ;
#6428 = ORIENTED_EDGE ( 'NONE', *, *, #2229, .F. ) ;
#6429 = CARTESIAN_POINT ( 'NONE',  ( -12.84969364742680753, -0.5881807229699745898, 36.82259397722437910 ) ) ;
#6430 = DIRECTION ( 'NONE',  ( 0.000000000000000000, 1.000000000000000000, 0.000000000000000000 ) ) ;
#6431 = DIRECTION ( 'NONE',  ( 0.000000000000000000, 0.000000000000000000, 1.000000000000000000 ) ) ;
#6432 = VERTEX_POINT ( 'NONE', #9457 ) ;
#6433 = CARTESIAN_POINT ( 'NONE',  ( -38.00000000000000711, 59.99999999999999289, -3.980288726281173287E-13 ) ) ;
#6434 = DIRECTION ( 'NONE',  ( 0.3286710990610907102, 0.000000000000000000, 0.9444444444444440867 ) ) ;
#6435 = ORIENTED_EDGE ( 'NONE', *, *, #5344, .T. ) ;
#6436 = DIRECTION ( 'NONE',  ( 0.000000000000000000, 0.7071067811865376918, 0.7071067811865573427 ) ) ;
#6437 = DIRECTION ( 'NONE',  ( -1.000000000000000000, 0.000000000000000000, 0.000000000000000000 ) ) ;
#6438 = CARTESIAN_POINT ( 'NONE',  ( 6.981204600336408994, 16.06533569283885399, 38.37097370016179809 ) ) ;
#6439 = LINE ( 'NONE', #9316, #803 ) ;
#6440 = DIRECTION ( 'NONE',  ( 0.000000000000000000, 0.000000000000000000, -1.000000000000000000 ) ) ;
#6441 = B_SPLINE_CURVE_WITH_KNOTS ( 'NONE', 3,
 ( #3157, #14, #9106, #3008 ),
 .UNSPECIFIED., .F., .F.,
 ( 4, 4 ),
 ( 9.813077866773594792E-18, 0.003679109433542027217 ),
 .UNSPECIFIED. ) ;
#6442 = ORIENTED_EDGE ( 'NONE', *, *, #411, .F. ) ;
#6443 = CARTESIAN_POINT ( 'NONE',  ( -10.00000000000001599, 3.294852476641298100, 184.6745183374407020 ) ) ;
#6444 = CARTESIAN_POINT ( 'NONE',  ( -5.562309845534584518, 69.99999999999998579, 33.06426808735054124 ) ) ;
#6445 = ORIENTED_EDGE ( 'NONE', *, *, #106, .T. ) ;
#6446 = DIRECTION ( 'NONE',  ( 1.735493991486223450E-29, 0.000000000000000000, -1.000000000000000000 ) ) ;
#6447 = FILL_AREA_STYLE_COLOUR ( '', #2457 ) ;
#6448 = AXIS2_PLACEMENT_3D ( 'NONE', #4220, #6611, #7261 ) ;
#6449 = ADVANCED_FACE ( 'NONE', ( #7778 ), #6696, .T. ) ;
#6450 = CARTESIAN_POINT ( 'NONE',  ( -8.545448575588370232, 56.50000000000029843, -24.55555555555557490 ) ) ;
#6451 = LINE ( 'NONE', #2798, #1622 ) ;
#6452 = AXIS2_PLACEMENT_3D ( 'NONE', #4386, #3587, #9610 ) ;
#6453 = DIRECTION ( 'NONE',  ( 0.000000000000000000, 0.000000000000000000, 1.000000000000000000 ) ) ;
#6454 = ORIENTED_EDGE ( 'NONE', *, *, #1473, .F. ) ;
#6455 = CARTESIAN_POINT ( 'NONE',  ( 1.193152119146780356E-26, 58.00000000000029132, -37.00000000000000711 ) ) ;
#6456 = CARTESIAN_POINT ( 'NONE',  ( -1.435128562976363265, -14.99999999999999822, 30.37910621253763566 ) ) ;
#6457 = VERTEX_POINT ( 'NONE', #7226 ) ;
#6458 = AXIS2_PLACEMENT_3D ( 'NONE', #4832, #7847, #1070 ) ;
#6459 = CARTESIAN_POINT ( 'NONE',  ( 1.300000000000000044, -0.7216878364870317197, -1.250000000000000000 ) ) ;
#6460 = DIRECTION ( 'NONE',  ( 0.000000000000000000, 0.000000000000000000, 1.000000000000000000 ) ) ;
#6461 = CARTESIAN_POINT ( 'NONE',  ( 2.216463206349838178, 13.07088745734695934, 38.96084410410938403 ) ) ;
#6462 =( NAMED_UNIT ( * ) SI_UNIT ( $, .STERADIAN. ) SOLID_ANGLE_UNIT ( ) );
#6463 = AXIS2_PLACEMENT_3D ( 'NONE', #4168, #6569, #4262 ) ;
#6464 = ADVANCED_FACE ( 'NONE', ( #7024 ), #9412, .F. ) ;
#6465 = CONICAL_SURFACE ( 'NONE', #2197, 26.00000000000000355, 0.7853981633974346233 ) ;
#6466 = ORIENTED_EDGE ( 'NONE', *, *, #4794, .T. ) ;
#6467 = CARTESIAN_POINT ( 'NONE',  ( -35.48172963891341425, 59.13032414405947179, -4.904055200121582025 ) ) ;
#6468 = VERTEX_POINT ( 'NONE', #2671 ) ;
#6469 = DIRECTION ( 'NONE',  ( -0.3286710990611142469, 0.000000000000000000, -0.9444444444444359821 ) ) ;
#6470 = ORIENTED_EDGE ( 'NONE', *, *, #988, .T. ) ;
#6471 = ORIENTED_EDGE ( 'NONE', *, *, #2617, .F. ) ;
#6472 = ADVANCED_FACE ( 'NONE', ( #3471 ), #6473, .F. ) ;
#6473 = CYLINDRICAL_SURFACE ( 'NONE', #1353, 1.500000000000001332 ) ;
#6474 =( GEOMETRIC_REPRESENTATION_CONTEXT ( 3 ) GLOBAL_UNCERTAINTY_ASSIGNED_CONTEXT ( ( #2616 ) ) GLOBAL_UNIT_ASSIGNED_CONTEXT ( ( #4951, #7368, #6462 ) ) REPRESENTATION_CONTEXT ( 'NONE', 'WORKASPACE' ) );
#6475 = EDGE_CURVE ( 'NONE', #2998, #4074, #3552, .T. ) ;
#6476 = DIRECTION ( 'NONE',  ( 0.000000000000000000, -1.000000000000000000, 0.000000000000000000 ) ) ;
#6477 = EDGE_CURVE ( 'NONE', #6561, #1456, #283, .T. ) ;
#6478 = VERTEX_POINT ( 'NONE', #8567 ) ;
#6479 = CARTESIAN_POINT ( 'NONE',  ( -10.23819876369190318, -5.532962098992985744, 37.64233965054218345 ) ) ;
#6480 = CARTESIAN_POINT ( 'NONE',  ( 29.00000000000000355, 30.00000000000000000, 5.000000000000000888 ) ) ;
#6481 =( GEOMETRIC_REPRESENTATION_CONTEXT ( 3 ) GLOBAL_UNCERTAINTY_ASSIGNED_CONTEXT ( ( #8655 ) ) GLOBAL_UNIT_ASSIGNED_CONTEXT ( ( #6806, #9046, #5291 ) ) REPRESENTATION_CONTEXT ( 'NONE', 'WORKASPACE' ) );
#6482 = EDGE_LOOP ( 'NONE', ( #2868, #2159, #6697, #8247, #4701 ) ) ;
#6483 = CARTESIAN_POINT ( 'NONE',  ( 4.000000000000001776, 30.00000000000000000, -29.00000000000000355 ) ) ;
#6484 = PLANE ( 'NONE',  #3300 ) ;
#6485 = EDGE_CURVE ( 'NONE', #6457, #4542, #1977, .T. ) ;
#6486 = PLANE ( 'NONE',  #809 ) ;
#6487 = CARTESIAN_POINT ( 'NONE',  ( 0.000000000000000000, 58.99999999999999289, -40.00000000000000711 ) ) ;
#6488 = AXIS2_PLACEMENT_3D ( 'NONE', #1334, #2018, #4304 ) ;
#6489 = VECTOR ( 'NONE', #3232, 1000.000000000000000 ) ;
#6490 = EDGE_CURVE ( 'NONE', #1519, #2516, #6542, .T. ) ;
#6491 = LINE ( 'NONE', #1807, #3389 ) ;
#6492 = ADVANCED_FACE ( 'NONE', ( #7974 ), #2520, .T. ) ;
#6493 = VECTOR ( 'NONE', #1640, 1000.000000000000000 ) ;
#6494 = EDGE_LOOP ( 'NONE', ( #4996, #4244, #4730, #9595 ) ) ;
#6495 = CARTESIAN_POINT ( 'NONE',  ( 1.040310318760209318E-26, 50.00000000000032685, -37.00000000000000711 ) ) ;
#6496 = CARTESIAN_POINT ( 'NONE',  ( 7.525660590371140657, 9.887872461981832117, 42.52846908860392716 ) ) ;
#6497 = ORIENTED_EDGE ( 'NONE', *, *, #237, .T. ) ;
#6498 = DIRECTION ( 'NONE',  ( 1.735493991486225972E-29, -6.508102468073347395E-30, -1.000000000000000000 ) ) ;
#6499 = FACE_OUTER_BOUND ( 'NONE', #6165, .T. ) ;
#6500 = CARTESIAN_POINT ( 'NONE',  ( 10.79742499427301894, 59.99999999999999289, -31.18357922838634977 ) ) ;
#6501 = CIRCLE ( 'NONE', #673, 27.99999999999999289 ) ;
#6502 = ADVANCED_FACE ( 'NONE', ( #7067 ), #3073, .T. ) ;
#6503 = AXIS2_PLACEMENT_3D ( 'NONE', #4447, #112, #3749 ) ;
#6504 = CARTESIAN_POINT ( 'NONE',  ( 8.982437128886548550, -6.367019354910812723, 38.05793569061005144 ) ) ;
#6505 = CARTESIAN_POINT ( 'NONE',  ( -23.54759692749571087, 39.99999999999999289, 18.58791755254458877 ) ) ;
#6506 = AXIS2_PLACEMENT_3D ( 'NONE', #4130, #5012, #6431 ) ;
#6507 = CARTESIAN_POINT ( 'NONE',  ( -33.06426808735054124, 61.99999999999999289, -5.562309845534586294 ) ) ;
#6508 = ADVANCED_FACE ( 'NONE', ( #6333 ), #1160, .F. ) ;
#6509 = VERTEX_POINT ( 'NONE', #8713 ) ;
#6510 = DIRECTION ( 'NONE',  ( 0.000000000000000000, -0.000000000000000000, 1.000000000000000000 ) ) ;
#6511 = CARTESIAN_POINT ( 'NONE',  ( -7.751339229931619279, -15.00000000000000355, 36.88905299132577653 ) ) ;
#6512 = VECTOR ( 'NONE', #4397, 1000.000000000000000 ) ;
#6513 = ORIENTED_EDGE ( 'NONE', *, *, #6721, .T. ) ;
#6514 = LINE ( 'NONE', #5039, #3494 ) ;
#6515 = CARTESIAN_POINT ( 'NONE',  ( -5.999999999999998224, -15.00000000000000000, 31.00000000000000711 ) ) ;
#6516 = CARTESIAN_POINT ( 'NONE',  ( 0.02451486834250751756, 18.29482697815594605, 38.99999229514322963 ) ) ;
#6517 = ORIENTED_EDGE ( 'NONE', *, *, #5138, .F. ) ;
#6518 = DIRECTION ( 'NONE',  ( 1.735493991486223450E-29, 0.000000000000000000, -1.000000000000000000 ) ) ;
#6519 = DIRECTION ( 'NONE',  ( 0.000000000000000000, 1.000000000000000000, 0.000000000000000000 ) ) ;
#6520 = CARTESIAN_POINT ( 'NONE',  ( 1.555535097482682654E-26, 78.08723716182652197, -25.00000000000000000 ) ) ;
#6521 = VERTEX_POINT ( 'NONE', #1939 ) ;
#6522 = ORIENTED_EDGE ( 'NONE', *, *, #166, .F. ) ;
#6523 = CARTESIAN_POINT ( 'NONE',  ( 0.01529561596030615950, 13.29484127273986260, 38.99999809024075148 ) ) ;
#6524 = CARTESIAN_POINT ( 'NONE',  ( 0.000000000000000000, -4.999999999999997335, 0.000000000000000000 ) ) ;
#6525 = EDGE_CURVE ( 'NONE', #6748, #8160, #8113, .T. ) ;
#6526 = CARTESIAN_POINT ( 'NONE',  ( 0.000000000000000000, 61.99999999999999289, 0.000000000000000000 ) ) ;
#6527 = AXIS2_PLACEMENT_3D ( 'NONE', #5079, #7399, #8188 ) ;
#6528 = VECTOR ( 'NONE', #5221, 1000.000000000000000 ) ;
#6529 = EDGE_LOOP ( 'NONE', ( #2756, #3695, #8537, #3379, #256 ) ) ;
#6530 = FACE_OUTER_BOUND ( 'NONE', #6919, .T. ) ;
#6531 = EDGE_CURVE ( 'NONE', #6561, #1760, #9085, .T. ) ;
#6532 = ORIENTED_EDGE ( 'NONE', *, *, #5585, .T. ) ;
#6533 = DIRECTION ( 'NONE',  ( 0.000000000000000000, 0.000000000000000000, -1.000000000000000000 ) ) ;
#6534 = AXIS2_PLACEMENT_3D ( 'NONE', #5497, #6363, #4162 ) ;
#6535 = DIRECTION ( 'NONE',  ( -1.000000000000000000, 0.000000000000000000, -1.047444401652941269E-14 ) ) ;
#6536 = AXIS2_PLACEMENT_3D ( 'NONE', #7987, #3485, #9514 ) ;
#6537 = CARTESIAN_POINT ( 'NONE',  ( 9.145707437616094282, 14.18749288135022368, 37.91311953629105602 ) ) ;
#6538 = LINE ( 'NONE', #537, #8373 ) ;
#6539 = FACE_OUTER_BOUND ( 'NONE', #5359, .T. ) ;
#6540 = CIRCLE ( 'NONE', #2275, 4.500000000000004441 ) ;
#6541 = AXIS2_PLACEMENT_3D ( 'NONE', #9200, #6862, #2412 ) ;
#6542 = CIRCLE ( 'NONE', #8457, 4.500000000000004441 ) ;
#6543 = CARTESIAN_POINT ( 'NONE',  ( 4.331874290630489455, 29.33187429063046991, -24.96033808169876878 ) ) ;
#6544 = EDGE_CURVE ( 'NONE', #2358, #7266, #1671, .T. ) ;
#6545 = EDGE_CURVE ( 'NONE', #3486, #3340, #3881, .T. ) ;
#6546 = ORIENTED_EDGE ( 'NONE', *, *, #1780, .F. ) ;
#6547 = FACE_OUTER_BOUND ( 'NONE', #932, .T. ) ;
#6548 = DIRECTION ( 'NONE',  ( 0.000000000000000000, -0.5000000000000000000, -0.8660254037844385966 ) ) ;
#6549 = EDGE_CURVE ( 'NONE', #7724, #9229, #3402, .T. ) ;
#6550 = CIRCLE ( 'NONE', #7177, 37.00000000000000711 ) ;
#6551 = ORIENTED_EDGE ( 'NONE', *, *, #8609, .T. ) ;
#6552 = CARTESIAN_POINT ( 'NONE',  ( -8.216777476527294510, 56.50000000000029843, -23.61111111111111427 ) ) ;
#6553 = LINE ( 'NONE', #8038, #5317 ) ;
#6554 = VECTOR ( 'NONE', #8306, 1000.000000000000000 ) ;
#6555 = CARTESIAN_POINT ( 'NONE',  ( 5.000000000000002665, 30.00000000000000000, 0.000000000000000000 ) ) ;
#6556 = VECTOR ( 'NONE', #5451, 1000.000000000000000 ) ;
#6557 = DIRECTION ( 'NONE',  ( 0.000000000000000000, 1.000000000000000000, 0.000000000000000000 ) ) ;
#6558 = VECTOR ( 'NONE', #6286, 1000.000000000000000 ) ;
#6559 = EDGE_CURVE ( 'NONE', #1992, #1652, #7010, .T. ) ;
#6560 = DIRECTION ( 'NONE',  ( 0.000000000000000000, 0.000000000000000000, -1.000000000000000000 ) ) ;
#6561 = VERTEX_POINT ( 'NONE', #1257 ) ;
#6562 = CARTESIAN_POINT ( 'NONE',  ( -5.562309845534584518, 59.99999999999999289, 33.06426808735054124 ) ) ;
#6563 = CARTESIAN_POINT ( 'NONE',  ( -2.136419886453954309, -9.299694386856355521, 39.45120225348325960 ) ) ;
#6564 = ORIENTED_EDGE ( 'NONE', *, *, #2987, .T. ) ;
#6565 = CIRCLE ( 'NONE', #4845, 2.500000000000002220 ) ;
#6566 = CARTESIAN_POINT ( 'NONE',  ( 9.762153702110021092E-27, 46.00000000000018474, -25.00000000000000000 ) ) ;
#6567 = PRODUCT_RELATED_PRODUCT_CATEGORY ( 'part', '', ( #2350 ) ) ;
#6568 = CARTESIAN_POINT ( 'NONE',  ( 8.807406495666141311, 14.57426945197969381, 37.99774521171899977 ) ) ;
#6569 = DIRECTION ( 'NONE',  ( 0.000000000000000000, 0.000000000000000000, 1.000000000000000000 ) ) ;
#6570 = ORIENTED_EDGE ( 'NONE', *, *, #7951, .T. ) ;
#6571 = CARTESIAN_POINT ( 'NONE',  ( -34.33638591132956464, 59.77059716828893698, -3.404146005973820888 ) ) ;
#6572 = ORIENTED_EDGE ( 'NONE', *, *, #8555, .T. ) ;
#6573 = CARTESIAN_POINT ( 'NONE',  ( 35.23154690738756756, 59.33548969180893806, 4.305939634252488268 ) ) ;
#6574 = ORIENTED_EDGE ( 'NONE', *, *, #1553, .F. ) ;
#6575 = DIRECTION ( 'NONE',  ( 1.820952055660014662E-28, 1.000000000000000000, 7.038118388768679669E-30 ) ) ;
#6576 = ORIENTED_EDGE ( 'NONE', *, *, #337, .F. ) ;
#6577 = CARTESIAN_POINT ( 'NONE',  ( -9.479506463030828556, 6.546681192253595682, 41.64102178833953616 ) ) ;
#6578 = DIRECTION ( 'NONE',  ( -0.000000000000000000, -1.000000000000000000, -0.000000000000000000 ) ) ;
#6579 = CARTESIAN_POINT ( 'NONE',  ( -8.216777476527294510, 53.50000000000031264, -23.61111111111107519 ) ) ;
#6580 = ORIENTED_EDGE ( 'NONE', *, *, #2017, .T. ) ;
#6581 = DIRECTION ( 'NONE',  ( -0.000000000000000000, 1.000000000000000000, -0.000000000000000000 ) ) ;
#6582 = DIRECTION ( 'NONE',  ( 0.000000000000000000, 1.000000000000000000, 0.000000000000000000 ) ) ;
#6583 = ORIENTED_EDGE ( 'NONE', *, *, #3112, .F. ) ;
#6584 = VERTEX_POINT ( 'NONE', #1352 ) ;
#6585 = DIRECTION ( 'NONE',  ( 0.3286710990610922090, 6.289316826390952918E-29, 0.9444444444444435316 ) ) ;
#6586 = DIRECTION ( 'NONE',  ( -0.000000000000000000, -0.000000000000000000, 1.000000000000000000 ) ) ;
#6587 = CARTESIAN_POINT ( 'NONE',  ( 0.000000000000000000, 39.99999999999999289, 0.000000000000000000 ) ) ;
#6588 = DIRECTION ( 'NONE',  ( -0.000000000000000000, -1.000000000000000000, -0.000000000000000000 ) ) ;
#6589 = CARTESIAN_POINT ( 'NONE',  ( -4.331874290630493007, 29.33187429063046991, -24.96033808169876878 ) ) ;
#6590 = ORIENTED_EDGE ( 'NONE', *, *, #7387, .F. ) ;
#6591 = CARTESIAN_POINT ( 'NONE',  ( 8.776077570583756335E-27, 49.00000000000032685, -24.09806918451531033 ) ) ;
#6592 = CARTESIAN_POINT ( 'NONE',  ( 1.675417577077328968, 13.15907318124163616, 43.93088470327393225 ) ) ;
#6593 = EDGE_LOOP ( 'NONE', ( #1449, #6570, #2567, #7327, #5142 ) ) ;
#6594 = LINE ( 'NONE', #9522, #7760 ) ;
#6595 = CARTESIAN_POINT ( 'NONE',  ( -5.999999999999998224, 27.42469319230601243, 31.00000000000000711 ) ) ;
#6596 = CARTESIAN_POINT ( 'NONE',  ( 4.336808689942017736E-16, 0.000000000000000000, 0.000000000000000000 ) ) ;
#6597 = ADVANCED_FACE ( 'NONE', ( #7426 ), #2167, .F. ) ;
#6598 = EDGE_CURVE ( 'NONE', #9443, #8766, #3617, .T. ) ;
#6599 = DIRECTION ( 'NONE',  ( 0.000000000000000000, 0.000000000000000000, 1.000000000000000000 ) ) ;
#6600 = ORIENTED_EDGE ( 'NONE', *, *, #2255, .F. ) ;
#6601 = CARTESIAN_POINT ( 'NONE',  ( 0.02042900839392215728, 18.29483547775932095, 38.99999486345961941 ) ) ;
#6602 = CARTESIAN_POINT ( 'NONE',  ( -7.537816291435827765, -14.99999999999999822, 28.01273613541154361 ) ) ;
#6603 = ORIENTED_EDGE ( 'NONE', *, *, #8179, .T. ) ;
#6604 = ADVANCED_FACE ( 'NONE', ( #3668 ), #4318, .T. ) ;
#6605 = LINE ( 'NONE', #5868, #39 ) ;
#6606 = VECTOR ( 'NONE', #3364, 1000.000000000000341 ) ;
#6607 = CIRCLE ( 'NONE', #5973, 4.500000000000005329 ) ;
#6608 = DIRECTION ( 'NONE',  ( 0.000000000000000000, -0.000000000000000000, 1.000000000000000000 ) ) ;
#6609 = ORIENTED_EDGE ( 'NONE', *, *, #5704, .T. ) ;
#6610 = ADVANCED_FACE ( 'NONE', ( #5011 ), #2778, .F. ) ;
#6611 = DIRECTION ( 'NONE',  ( 0.000000000000000000, 1.000000000000000000, 0.000000000000000000 ) ) ;
#6612 = CONTEXT_DEPENDENT_SHAPE_REPRESENTATION ( #5119, #173 ) ;
#6613 = VERTEX_POINT ( 'NONE', #2078 ) ;
#6614 = LINE ( 'NONE', #8897, #7178 ) ;
#6615 = ORIENTED_EDGE ( 'NONE', *, *, #6001, .F. ) ;
#6616 = CARTESIAN_POINT ( 'NONE',  ( 35.30849208807571671, 59.27954177615072240, 4.448983360113043517 ) ) ;
#6617 = ORIENTED_EDGE ( 'NONE', *, *, #8714, .T. ) ;
#6618 = LINE ( 'NONE', #8632, #6084 ) ;
#6619 = CIRCLE ( 'NONE', #1269, 27.99999999999999289 ) ;
#6620 = VERTEX_POINT ( 'NONE', #2919 ) ;
#6621 = CARTESIAN_POINT ( 'NONE',  ( -11.51340233387757017, 10.85928029369878267, 37.26517847978107767 ) ) ;
#6622 = CARTESIAN_POINT ( 'NONE',  ( -33.06426808735054124, 69.99999999999998579, -5.562309845534581854 ) ) ;
#6623 = ORIENTED_EDGE ( 'NONE', *, *, #5990, .F. ) ;
#6624 = CARTESIAN_POINT ( 'NONE',  ( -28.87459861216645862, 60.99999999999999289, -15.97678174684361707 ) ) ;
#6625 = ORIENTED_EDGE ( 'NONE', *, *, #8287, .T. ) ;
#6626 = DIRECTION ( 'NONE',  ( 0.000000000000000000, 0.000000000000000000, 1.000000000000000000 ) ) ;
#6627 = EDGE_CURVE ( 'NONE', #8321, #4095, #7269, .T. ) ;
#6628 = CARTESIAN_POINT ( 'NONE',  ( 1.555535097482682654E-26, 78.08723716182652197, -25.00000000000000000 ) ) ;
#6629 = DIRECTION ( 'NONE',  ( 1.735493991486225972E-29, -6.508102468073347395E-30, -1.000000000000000000 ) ) ;
#6630 = LINE ( 'NONE', #1504, #5283 ) ;
#6631 = PRODUCT_DEFINITION_FORMATION_WITH_SPECIFIED_SOURCE ( 'ANY', '', #2350, .NOT_KNOWN. ) ;
#6632 = CARTESIAN_POINT ( 'NONE',  ( -4.000000000000005329, 28.99999999999997158, -24.67792535850613334 ) ) ;
#6633 = ORIENTED_EDGE ( 'NONE', *, *, #2488, .T. ) ;
#6634 = DIRECTION ( 'NONE',  ( -0.3286710990610922090, -6.289316826390952918E-29, -0.9444444444444435316 ) ) ;
#6635 = DIRECTION ( 'NONE',  ( -1.820952055660014662E-28, -1.000000000000000000, -7.038118388768679669E-30 ) ) ;
#6636 = CARTESIAN_POINT ( 'NONE',  ( 0.000000000000000000, 61.99999999999999289, 0.000000000000000000 ) ) ;
#6637 = AXIS2_PLACEMENT_3D ( 'NONE', #7887, #6342, #6886 ) ;
#6638 = CARTESIAN_POINT ( 'NONE',  ( 9.269115636346888714E-27, 44.00000000000019895, -37.00000000000000711 ) ) ;
#6639 = DIRECTION ( 'NONE',  ( -1.084202172485503325E-16, 0.000000000000000000, -1.000000000000000000 ) ) ;
#6640 = CARTESIAN_POINT ( 'NONE',  ( -31.00000000000000355, 27.99909559099847911, -2.017392264862527096 ) ) ;
#6641 = EDGE_CURVE ( 'NONE', #3567, #4855, #2755, .T. ) ;
#6642 = AXIS2_PLACEMENT_3D ( 'NONE', #7109, #1782, #6320 ) ;
#6643 = CARTESIAN_POINT ( 'NONE',  ( 1.555535097482682654E-26, 78.08723716182652197, -25.00000000000000000 ) ) ;
#6644 = DIRECTION ( 'NONE',  ( -0.000000000000000000, -1.000000000000000000, -0.000000000000000000 ) ) ;
#6645 = VERTEX_POINT ( 'NONE', #1444 ) ;
#6646 = CARTESIAN_POINT ( 'NONE',  ( 4.898587196589413815E-15, 39.99999999999999289, 40.00000000000000711 ) ) ;
#6647 = CARTESIAN_POINT ( 'NONE',  ( 8.323710113664041899, -6.781460580756969669, 38.26155278793961401 ) ) ;
#6648 = VECTOR ( 'NONE', #2198, 1000.000000000000000 ) ;
#6649 = EDGE_CURVE ( 'NONE', #8408, #1910, #8768, .T. ) ;
#6650 = ORIENTED_EDGE ( 'NONE', *, *, #4145, .F. ) ;
#6651 = CARTESIAN_POINT ( 'NONE',  ( 9.469456053449529731E-27, 52.00000000000031974, 3.146969529128743384E-28 ) ) ;
#6652 = DIRECTION ( 'NONE',  ( -1.000000000000000000, -0.000000000000000000, -0.000000000000000000 ) ) ;
#6653 = ORIENTED_EDGE ( 'NONE', *, *, #6205, .F. ) ;
#6654 = AXIS2_PLACEMENT_3D ( 'NONE', #4049, #5572, #5526 ) ;
#6655 = CARTESIAN_POINT ( 'NONE',  ( 8.908588037261978343, 7.879430400622490005, 38.11900311772433270 ) ) ;
#6656 = ITEM_DEFINED_TRANSFORMATION ( 'NONE', 'NONE', #9007,  #6314 ) ;
#6657 = ORIENTED_EDGE ( 'NONE', *, *, #9459, .F. ) ;
#6658 = CARTESIAN_POINT ( 'NONE',  ( -35.30849208807571671, 59.27954177615072240, -4.448983360113034635 ) ) ;
#6659 = EDGE_CURVE ( 'NONE', #7105, #2210, #258, .T. ) ;
#6660 = VERTEX_POINT ( 'NONE', #713 ) ;
#6661 = CARTESIAN_POINT ( 'NONE',  ( 35.56420151578587507, 58.98289357006406419, 5.732470078048714335 ) ) ;
#6662 = EDGE_CURVE ( 'NONE', #7666, #6561, #7828, .T. ) ;
#6663 = VERTEX_POINT ( 'NONE', #3518 ) ;
#6664 = CARTESIAN_POINT ( 'NONE',  ( 0.000000000000000000, 59.99999999999999289, 0.000000000000000000 ) ) ;
#6665 = EDGE_CURVE ( 'NONE', #504, #6918, #4045, .T. ) ;
#6666 = ORIENTED_EDGE ( 'NONE', *, *, #5030, .T. ) ;
#6667 = CARTESIAN_POINT ( 'NONE',  ( -2.597462001549401212, 12.97425228067757175, 43.83800940528956858 ) ) ;
#6668 = DIRECTION ( 'NONE',  ( 0.000000000000000000, 0.000000000000000000, 1.000000000000000000 ) ) ;
#6669 = CARTESIAN_POINT ( 'NONE',  ( -6.000000000000005329, 27.42469319230600533, -31.00000000000000711 ) ) ;
#6670 = ORIENTED_EDGE ( 'NONE', *, *, #1180, .F. ) ;
#6671 = DIRECTION ( 'NONE',  ( 0.5773502691896205130, 0.5773502691896365002, 0.5773502691896204020 ) ) ;
#6672 = DIRECTION ( 'NONE',  ( -0.3286710990611015903, 0.000000000000000000, -0.9444444444444403119 ) ) ;
#6673 = ORIENTED_EDGE ( 'NONE', *, *, #6152, .T. ) ;
#6674 = DIRECTION ( 'NONE',  ( 0.000000000000000000, -0.000000000000000000, -1.000000000000000000 ) ) ;
#6675 = DIRECTION ( 'NONE',  ( 1.000000000000000000, -0.000000000000000000, 0.000000000000000000 ) ) ;
#6676 = SURFACE_SIDE_STYLE ('',( #2140 ) ) ;
#6677 = AXIS2_PLACEMENT_3D ( 'NONE', #4288, #7993, #1275 ) ;
#6678 = CARTESIAN_POINT ( 'NONE',  ( 8.677469957431129860E-27, 40.00000000000014921, -25.00000000000000000 ) ) ;
#6679 = CARTESIAN_POINT ( 'NONE',  ( 29.00000000000000355, 0.000000000000000000, -4.000000000000007105 ) ) ;
#6680 = ORIENTED_EDGE ( 'NONE', *, *, #3220, .T. ) ;
#6681 = CIRCLE ( 'NONE', #3537, 1.500000000000001332 ) ;
#6682 = DIRECTION ( 'NONE',  ( 0.000000000000000000, 0.000000000000000000, -1.000000000000000000 ) ) ;
#6683 = CARTESIAN_POINT ( 'NONE',  ( 1.555535097482682654E-26, 78.08723716182652197, -25.00000000000000000 ) ) ;
#6684 = CARTESIAN_POINT ( 'NONE',  ( 1.820000000000000062, 0.000000000000000000, 0.000000000000000000 ) ) ;
#6685 = CARTESIAN_POINT ( 'NONE',  ( 4.817158075008645568, -15.00000000000000178, 29.05778733718146611 ) ) ;
#6686 = CARTESIAN_POINT ( 'NONE',  ( 30.12488991936162108, 28.28385863652523824, -6.000000000000006217 ) ) ;
#6687 = CARTESIAN_POINT ( 'NONE',  ( -2.254158640986140050, 18.08224550467000569, 38.93613429042778051 ) ) ;
#6688 = CIRCLE ( 'NONE', #8595, 1.500000000000001332 ) ;
#6689 = AXIS2_PLACEMENT_3D ( 'NONE', #6970, #5510, #6827 ) ;
#6690 = CARTESIAN_POINT ( 'NONE',  ( 30.00000000000000711, 30.00000000000000000, -5.000000000000007994 ) ) ;
#6691 = VECTOR ( 'NONE', #8154, 1000.000000000000000 ) ;
#6692 = FACE_BOUND ( 'NONE', #922, .T. ) ;
#6693 = CIRCLE ( 'NONE', #4517, 5.000000000000000888 ) ;
#6694 = PLANE ( 'NONE',  #5587 ) ;
#6695 = AXIS2_PLACEMENT_3D ( 'NONE', #8733, #1956, #4977 ) ;
#6696 = TOROIDAL_SURFACE ( 'NONE', #1822, 33.00000000000000711, 5.000000000000000000 ) ;
#6697 = ORIENTED_EDGE ( 'NONE', *, *, #9513, .F. ) ;
#6698 = LINE ( 'NONE', #9727, #4160 ) ;
#6699 = CARTESIAN_POINT ( 'NONE',  ( 7.536687028107835751, -15.00000000000000000, 28.01307067288326280 ) ) ;
#6700 = EDGE_LOOP ( 'NONE', ( #4123, #9517, #2165, #4828 ) ) ;
#6701 = LINE ( 'NONE', #8987, #6648 ) ;
#6702 = AXIS2_PLACEMENT_3D ( 'NONE', #567, #8901, #707 ) ;
#6703 = CARTESIAN_POINT ( 'NONE',  ( -29.00000000000000355, 28.99999999999997158, 0.000000000000000000 ) ) ;
#6704 = VERTEX_POINT ( 'NONE', #8808 ) ;
#6705 = ADVANCED_FACE ( 'NONE', ( #572 ), #9556, .T. ) ;
#6706 = CARTESIAN_POINT ( 'NONE',  ( 11.91013294755531149, -3.389816855901808701, 37.13751894432687806 ) ) ;
#6707 = APPLICATION_PROTOCOL_DEFINITION ( 'draft international standard', 'automotive_design', 1998, #9160 ) ;
#6708 = ORIENTED_EDGE ( 'NONE', *, *, #1792, .F. ) ;
#6709 = VERTEX_POINT ( 'NONE', #4561 ) ;
#6710 = DIRECTION ( 'NONE',  ( -0.9860132971832693549, -1.788557213313974126E-28, 0.1666666666666657970 ) ) ;
#6711 = CIRCLE ( 'NONE', #7362, 33.00000000000000711 ) ;
#6712 = ORIENTED_EDGE ( 'NONE', *, *, #3282, .F. ) ;
#6713 = DIRECTION ( 'NONE',  ( -1.820952055660014662E-28, -1.000000000000000000, -7.038118388768679669E-30 ) ) ;
#6714 = EDGE_LOOP ( 'NONE', ( #1289, #527, #4389, #9266 ) ) ;
#6715 = DIRECTION ( 'NONE',  ( 1.820952055660014662E-28, 1.000000000000000000, -6.508102468073347395E-30 ) ) ;
#6716 = ORIENTED_EDGE ( 'NONE', *, *, #5719, .F. ) ;
#6717 = DIRECTION ( 'NONE',  ( 0.000000000000000000, -0.7071067811865500152, -0.7071067811865451302 ) ) ;
#6718 = DIRECTION ( 'NONE',  ( 0.000000000000000000, 0.000000000000000000, 1.000000000000000000 ) ) ;
#6719 = DIRECTION ( 'NONE',  ( -1.820952055660014662E-28, -1.000000000000000000, -7.038118388768679669E-30 ) ) ;
#6720 = EDGE_CURVE ( 'NONE', #1969, #9011, #9113, .T. ) ;
#6721 = EDGE_CURVE ( 'NONE', #5636, #7720, #5352, .T. ) ;
#6722 = ADVANCED_FACE ( 'NONE', ( #2415 ), #3062, .F. ) ;
#6723 = AXIS2_PLACEMENT_3D ( 'NONE', #6591, #5856, #1411 ) ;
#6724 = ORIENTED_EDGE ( 'NONE', *, *, #8665, .F. ) ;
#6725 = CARTESIAN_POINT ( 'NONE',  ( -5.044664205793679024, -8.473593863896581979, 39.07304412537308025 ) ) ;
#6726 = DIRECTION ( 'NONE',  ( -0.000000000000000000, -1.000000000000000000, -0.000000000000000000 ) ) ;
#6727 = CARTESIAN_POINT ( 'NONE',  ( 0.000000000000000000, 59.99999999999999289, 0.000000000000000000 ) ) ;
#6728 = CARTESIAN_POINT ( 'NONE',  ( 6.439978105601112524E-15, 18.29485247664131009, 39.00000000000002132 ) ) ;
#6729 = CARTESIAN_POINT ( 'NONE',  ( -33.06426808735054124, 59.99576382555915899, -3.062309845534580077 ) ) ;
#6730 = EDGE_CURVE ( 'NONE', #7154, #6767, #3921, .T. ) ;
#6731 = DIRECTION ( 'NONE',  ( -0.000000000000000000, 0.5000000000000000000, 0.8660254037844385966 ) ) ;
#6732 = ORIENTED_EDGE ( 'NONE', *, *, #2828, .T. ) ;
#6733 = CARTESIAN_POINT ( 'NONE',  ( 0.000000000000000000, 19.99999999999982236, 0.000000000000000000 ) ) ;
#6734 = DIRECTION ( 'NONE',  ( 0.000000000000000000, 0.000000000000000000, -1.000000000000000000 ) ) ;
#6735 = DIRECTION ( 'NONE',  ( 0.000000000000000000, -0.000000000000000000, 1.000000000000000000 ) ) ;
#6736 = DIRECTION ( 'NONE',  ( -0.000000000000000000, 0.000000000000000000, 1.000000000000000000 ) ) ;
#6737 = CARTESIAN_POINT ( 'NONE',  ( 1.057802637207955558E-26, 58.00000000000029132, 3.077636051130802893E-28 ) ) ;
#6738 = CARTESIAN_POINT ( 'NONE',  ( -2.575401375589585040, 18.01522921748959405, 38.91614804012162665 ) ) ;
#6739 = ADVANCED_FACE ( 'NONE', ( #8362 ), #8464, .T. ) ;
#6740 = FACE_OUTER_BOUND ( 'NONE', #3370, .T. ) ;
#6741 = CARTESIAN_POINT ( 'NONE',  ( 4.898587196589413815E-15, 37.99999999999996447, 40.00000000000000711 ) ) ;
#6742 = EDGE_LOOP ( 'NONE', ( #2307, #4266, #5508, #7566, #3704, #5347, #9048, #7365, #5500, #4673, #227 ) ) ;
#6743 = PLANE ( 'NONE',  #9507 ) ;
#6744 = CARTESIAN_POINT ( 'NONE',  ( 0.8972019483868172163, -15.00000000000000000, 30.49724507882217495 ) ) ;
#6745 = ORIENTED_EDGE ( 'NONE', *, *, #3964, .F. ) ;
#6746 = CARTESIAN_POINT ( 'NONE',  ( 1.148778693228098442E-26, 59.00000000000029843, -24.09806918451521440 ) ) ;
#6747 = CARTESIAN_POINT ( 'NONE',  ( 0.000000000000000000, 3.294852476641296768, 184.6745183374407020 ) ) ;
#6748 = VERTEX_POINT ( 'NONE', #132 ) ;
#6749 = CARTESIAN_POINT ( 'NONE',  ( 9.098375990985465123, -0.8675798692180576310, 41.83041446991980905 ) ) ;
#6750 = EDGE_LOOP ( 'NONE', ( #2459, #316, #3603, #231 ) ) ;
#6751 = CARTESIAN_POINT ( 'NONE',  ( -24.67792535850613334, 28.99999999999997158, -3.999999999999997335 ) ) ;
#6752 = DIRECTION ( 'NONE',  ( -0.000000000000000000, 1.000000000000000000, -0.000000000000000000 ) ) ;
#6753 = DIRECTION ( 'NONE',  ( -0.3271946967961539277, 0.000000000000000000, 0.9449569463147370341 ) ) ;
#6754 = ORIENTED_EDGE ( 'NONE', *, *, #4265, .T. ) ;
#6755 = DIRECTION ( 'NONE',  ( 0.000000000000000000, 1.000000000000000000, 0.000000000000000000 ) ) ;
#6756 = ORIENTED_EDGE ( 'NONE', *, *, #4275, .F. ) ;
#6757 = LINE ( 'NONE', #3720, #8909 ) ;
#6758 = VECTOR ( 'NONE', #946, 1000.000000000000000 ) ;
#6759 = CIRCLE ( 'NONE', #8681, 30.00000000000001066 ) ;
#6760 = CARTESIAN_POINT ( 'NONE',  ( 1.084683744678891232E-26, 58.00000000000029132, -24.09806918451521440 ) ) ;
#6761 = CARTESIAN_POINT ( 'NONE',  ( -2.318347576506052388, -6.438274054832179516, 43.86504657511039085 ) ) ;
#6762 = EDGE_CURVE ( 'NONE', #9346, #1074, #2859, .T. ) ;
#6763 = ADVANCED_FACE ( 'NONE', ( #4710 ), #4617, .F. ) ;
#6764 = AXIS2_PLACEMENT_3D ( 'NONE', #8523, #4964, #7883 ) ;
#6765 = VERTEX_POINT ( 'NONE', #7620 ) ;
#6766 = CARTESIAN_POINT ( 'NONE',  ( -8.070750150710590987, 59.89221580632704445, 33.08193339022353285 ) ) ;
#6767 = VERTEX_POINT ( 'NONE', #807 ) ;
#6768 = EDGE_CURVE ( 'NONE', #1665, #7105, #6022, .T. ) ;
#6769 = ORIENTED_EDGE ( 'NONE', *, *, #1848, .T. ) ;
#6770 = FACE_OUTER_BOUND ( 'NONE', #3365, .T. ) ;
#6771 = FACE_OUTER_BOUND ( 'NONE', #5932, .T. ) ;
#6772 = ADVANCED_FACE ( 'NONE', ( #6816 ), #860, .T. ) ;
#6773 = CARTESIAN_POINT ( 'NONE',  ( -29.00000000000000355, 28.99999999999997158, -3.999999999999996447 ) ) ;
#6774 = AXIS2_PLACEMENT_3D ( 'NONE', #7788, #9469, #4041 ) ;
#6775 = DIRECTION ( 'NONE',  ( -1.820952055660014662E-28, -1.000000000000000000, -7.038118388768679669E-30 ) ) ;
#6776 = ADVANCED_FACE ( 'NONE', ( #7674 ), #7716, .T. ) ;
#6777 = ORIENTED_EDGE ( 'NONE', *, *, #9508, .T. ) ;
#6778 = FACE_OUTER_BOUND ( 'NONE', #9054, .T. ) ;
#6779 = DIRECTION ( 'NONE',  ( -0.000000000000000000, -1.000000000000000000, -0.000000000000000000 ) ) ;
#6780 = EDGE_CURVE ( 'NONE', #2072, #7884, #1615, .T. ) ;
#6781 =( GEOMETRIC_REPRESENTATION_CONTEXT ( 3 ) GLOBAL_UNCERTAINTY_ASSIGNED_CONTEXT ( ( #2277 ) ) GLOBAL_UNIT_ASSIGNED_CONTEXT ( ( #147, #4728, #9226 ) ) REPRESENTATION_CONTEXT ( 'NONE', 'WORKASPACE' ) );
#6782 = EDGE_LOOP ( 'NONE', ( #4836, #6849, #3961, #4768 ) ) ;
#6783 = DIRECTION ( 'NONE',  ( 0.3286710990610922090, 6.289316826390952918E-29, 0.9444444444444435316 ) ) ;
#6784 = CARTESIAN_POINT ( 'NONE',  ( 5.562309845534588959, 60.99999999999999289, -33.06426808735054124 ) ) ;
#6785 = EDGE_CURVE ( 'NONE', #4852, #1097, #8178, .T. ) ;
#6786 = DIRECTION ( 'NONE',  ( 0.000000000000000000, 1.000000000000000000, 0.000000000000000000 ) ) ;
#6787 = CARTESIAN_POINT ( 'NONE',  ( 9.762153702110021092E-27, 42.50000000000020606, -37.00000000000000711 ) ) ;
#6788 = ADVANCED_FACE ( 'NONE', ( #3966, #5306 ), #2212, .F. ) ;
#6789 = DIRECTION ( 'NONE',  ( 1.735493991486227934E-29, 0.000000000000000000, -1.000000000000000000 ) ) ;
#6790 = ORIENTED_EDGE ( 'NONE', *, *, #8570, .T. ) ;
#6791 = EDGE_CURVE ( 'NONE', #1432, #5694, #4620, .T. ) ;
#6792 = CARTESIAN_POINT ( 'NONE',  ( -31.00000000000000711, 30.00000000000000000, -5.999999999999996447 ) ) ;
#6793 = VECTOR ( 'NONE', #3181, 1000.000000000000000 ) ;
#6794 = DIRECTION ( 'NONE',  ( 0.000000000000000000, 0.000000000000000000, -1.000000000000000000 ) ) ;
#6795 = DIRECTION ( 'NONE',  ( 1.000000000000000000, 0.000000000000000000, 0.000000000000000000 ) ) ;
#6796 = VERTEX_POINT ( 'NONE', #3013 ) ;
#6797 = DIRECTION ( 'NONE',  ( -0.000000000000000000, -1.000000000000000000, -0.000000000000000000 ) ) ;
#6798 = CARTESIAN_POINT ( 'NONE',  ( 7.229529499415464855, -7.426880451839177333, 38.57586176292668512 ) ) ;
#6799 = VERTEX_POINT ( 'NONE', #9056 ) ;
#6800 = AXIS2_PLACEMENT_3D ( 'NONE', #7869, #7006, #1874 ) ;
#6801 = DIRECTION ( 'NONE',  ( 3.552713678800500929E-15, 0.000000000000000000, 1.000000000000000000 ) ) ;
#6802 = APPLICATION_CONTEXT ( 'automotive_design' ) ;
#6803 = DIRECTION ( 'NONE',  ( -0.000000000000000000, 1.000000000000000000, -0.000000000000000000 ) ) ;
#6804 = EDGE_LOOP ( 'NONE', ( #1439, #4965, #6179, #6386 ) ) ;
#6805 = CARTESIAN_POINT ( 'NONE',  ( 9.920401881134884192, 4.597042934328839259, 41.40737016411131322 ) ) ;
#6806 =( LENGTH_UNIT ( ) NAMED_UNIT ( * ) SI_UNIT ( .MILLI., .METRE. ) );
#6807 = VECTOR ( 'NONE', #1011, 1000.000000000000000 ) ;
#6808 = ORIENTED_EDGE ( 'NONE', *, *, #7755, .T. ) ;
#6809 = CARTESIAN_POINT ( 'NONE',  ( 8.831777707322487581E-27, 48.50000000000033396, 2.950524674801245327E-28 ) ) ;
#6810 = CARTESIAN_POINT ( 'NONE',  ( -24.96033808169876878, 29.33187429063046991, 4.331874290630497448 ) ) ;
#6811 = CARTESIAN_POINT ( 'NONE',  ( -4.999999999999998224, 30.00000000000000000, 25.51470164434615029 ) ) ;
#6812 = ORIENTED_EDGE ( 'NONE', *, *, #1071, .T. ) ;
#6813 = CYLINDRICAL_SURFACE ( 'NONE', #9719, 26.00000000000004974 ) ;
#6814 = ORIENTED_EDGE ( 'NONE', *, *, #9268, .T. ) ;
#6815 = CARTESIAN_POINT ( 'NONE',  ( -1.639856434810980312, 13.16510872014126221, 43.93393704144139633 ) ) ;
#6816 = FACE_OUTER_BOUND ( 'NONE', #7421, .T. ) ;
#6817 = AXIS2_PLACEMENT_3D ( 'NONE', #7881, #7832, #9413 ) ;
#6818 = DIRECTION ( 'NONE',  ( 1.000000000000000000, 0.000000000000000000, 0.000000000000000000 ) ) ;
#6819 = AXIS2_PLACEMENT_3D ( 'NONE', #7142, #6302, #1719 ) ;
#6820 = EDGE_LOOP ( 'NONE', ( #7898, #2595, #218, #2726, #5551 ) ) ;
#6821 = CARTESIAN_POINT ( 'NONE',  ( -9.421158911257350610, -6.091526235802759537, 37.92262462108629961 ) ) ;
#6822 = ORIENTED_EDGE ( 'NONE', *, *, #3050, .T. ) ;
#6823 = CIRCLE ( 'NONE', #4317, 37.99999999999999289 ) ;
#6824 = ORIENTED_EDGE ( 'NONE', *, *, #2500, .F. ) ;
#6825 = CARTESIAN_POINT ( 'NONE',  ( 0.000000000000000000, 0.000000000000000000, 0.000000000000000000 ) ) ;
#6826 = ADVANCED_FACE ( 'NONE', ( #7160 ), #6369, .F. ) ;
#6827 = DIRECTION ( 'NONE',  ( -0.9860132971832694659, -1.788557213313974350E-28, 0.1666666666666658247 ) ) ;
#6828 = DIRECTION ( 'NONE',  ( 0.000000000000000000, -0.000000000000000000, 1.000000000000000000 ) ) ;
#6829 = EDGE_LOOP ( 'NONE', ( #2963, #754, #6532, #6653 ) ) ;
#6830 = FACE_OUTER_BOUND ( 'NONE', #6162, .T. ) ;
#6831 = ORIENTED_EDGE ( 'NONE', *, *, #9297, .T. ) ;
#6832 = CARTESIAN_POINT ( 'NONE',  ( 9.934199572794879529, 1.970741329907451878, 41.40042185314993617 ) ) ;
#6833 = CARTESIAN_POINT ( 'NONE',  ( 34.07933880998927378, 60.99999999999999289, -5.371095444502794081 ) ) ;
#6834 = DIRECTION ( 'NONE',  ( 0.5773502691896204020, 0.5773502691896366112, -0.5773502691896204020 ) ) ;
#6835 = CARTESIAN_POINT ( 'NONE',  ( -5.492748336992913316, -15.00000000000000000, 28.77311788903328704 ) ) ;
#6836 = PLANE ( 'NONE',  #5631 ) ;
#6837 = AXIS2_PLACEMENT_3D ( 'NONE', #3590, #3539, #6548 ) ;
#6838 = DIRECTION ( 'NONE',  ( -0.000000000000000000, 1.000000000000000000, -0.000000000000000000 ) ) ;
#6839 = DIRECTION ( 'NONE',  ( -0.000000000000000000, -1.000000000000000000, -0.000000000000000000 ) ) ;
#6840 = ADVANCED_FACE ( 'NONE', ( #7212 ), #4458, .T. ) ;
#6841 = ADVANCED_FACE ( 'NONE', ( #3311 ), #4853, .T. ) ;
#6842 = CIRCLE ( 'NONE', #3385, 30.00000000000001066 ) ;
#6843 = EDGE_CURVE ( 'NONE', #4855, #3567, #3819, .T. ) ;
#6844 = CARTESIAN_POINT ( 'NONE',  ( 0.000000000000000000, -10.00000000000000533, 0.000000000000000000 ) ) ;
#6845 = CARTESIAN_POINT ( 'NONE',  ( 4.336808689942017736E-16, -0.7216878364870318308, 1.250000000000000000 ) ) ;
#6846 = ORIENTED_EDGE ( 'NONE', *, *, #2808, .T. ) ;
#6847 = CARTESIAN_POINT ( 'NONE',  ( -8.216777476527294510, 45.50000000000019185, -23.61111111111111427 ) ) ;
#6848 = CARTESIAN_POINT ( 'NONE',  ( 1.773160951616444825, -14.99999999999999822, 30.27161250924837432 ) ) ;
#6849 = ORIENTED_EDGE ( 'NONE', *, *, #6261, .T. ) ;
#6850 = CIRCLE ( 'NONE', #5131, 33.00000000000000711 ) ;
#6851 =( GEOMETRIC_REPRESENTATION_CONTEXT ( 3 ) GLOBAL_UNCERTAINTY_ASSIGNED_CONTEXT ( ( #4570 ) ) GLOBAL_UNIT_ASSIGNED_CONTEXT ( ( #2176, #723, #4677 ) ) REPRESENTATION_CONTEXT ( 'NONE', 'WORKASPACE' ) );
#6852 = CARTESIAN_POINT ( 'NONE',  ( -28.87459861216645862, 61.99999999999999289, -15.97678174684361707 ) ) ;
#6853 = CARTESIAN_POINT ( 'NONE',  ( 3.517955418139624424, 61.99189485091271479, -37.07865250164482518 ) ) ;
#6854 = VERTEX_POINT ( 'NONE', #3418 ) ;
#6855 = VECTOR ( 'NONE', #59, 1000.000000000000000 ) ;
#6856 = AXIS2_PLACEMENT_3D ( 'NONE', #4071, #2622, #2664 ) ;
#6857 = CARTESIAN_POINT ( 'NONE',  ( 12.09670444263329081, -2.948796042164175457, 37.07695828027222973 ) ) ;
#6858 = CIRCLE ( 'NONE', #8133, 38.00000000000000711 ) ;
#6859 = VECTOR ( 'NONE', #6280, 1000.000000000000000 ) ;
#6860 = EDGE_LOOP ( 'NONE', ( #100, #9164, #3452, #6159 ) ) ;
#6861 = CARTESIAN_POINT ( 'NONE',  ( 1.148778693228098442E-26, 55.00000000000030553, -25.00000000000000000 ) ) ;
#6862 = DIRECTION ( 'NONE',  ( 0.7071067811865573427, 0.7071067811865376918, 0.000000000000000000 ) ) ;
#6863 = ORIENTED_EDGE ( 'NONE', *, *, #7582, .T. ) ;
#6864 = DIRECTION ( 'NONE',  ( -0.9860132971832693549, -1.787355433028676715E-28, 0.1666666666666661856 ) ) ;
#6865 = ORIENTED_EDGE ( 'NONE', *, *, #5354, .F. ) ;
#6866 = LINE ( 'NONE', #7525, #5590 ) ;
#6867 = AXIS2_PLACEMENT_3D ( 'NONE', #1479, #752, #9145 ) ;
#6868 = AXIS2_PLACEMENT_3D ( 'NONE', #4471, #2727, #9555 ) ;
#6869 = DIRECTION ( 'NONE',  ( -2.168404344971006649E-16, 0.000000000000000000, -1.000000000000000000 ) ) ;
#6870 = DIRECTION ( 'NONE',  ( 0.000000000000000000, 1.000000000000000000, 0.000000000000000000 ) ) ;
#6871 = AXIS2_PLACEMENT_3D ( 'NONE', #8536, #1764, #6354 ) ;
#6872 = ORIENTED_EDGE ( 'NONE', *, *, #4694, .F. ) ;
#6873 = CARTESIAN_POINT ( 'NONE',  ( 1.193152119146780356E-26, 56.00000000000030553, -37.00000000000000711 ) ) ;
#6874 = ORIENTED_EDGE ( 'NONE', *, *, #4492, .F. ) ;
#6875 = ORIENTED_EDGE ( 'NONE', *, *, #8665, .T. ) ;
#6876 = CARTESIAN_POINT ( 'NONE',  ( 4.000000000000002665, 28.99999999999997158, -8.673617379884032514E-16 ) ) ;
#6877 = DIRECTION ( 'NONE',  ( -1.000000000000000000, 0.000000000000000000, 0.000000000000000000 ) ) ;
#6878 = AXIS2_PLACEMENT_3D ( 'NONE', #7900, #595, #7996 ) ;
#6879 = DIRECTION ( 'NONE',  ( 0.000000000000000000, -1.000000000000000000, 0.000000000000000000 ) ) ;
#6880 = ORIENTED_EDGE ( 'NONE', *, *, #6913, .F. ) ;
#6881 = LINE ( 'NONE', #8378, #5054 ) ;
#6882 = DIRECTION ( 'NONE',  ( 0.000000000000000000, 0.000000000000000000, 1.000000000000000000 ) ) ;
#6883 = VERTEX_POINT ( 'NONE', #5588 ) ;
#6884 = CARTESIAN_POINT ( 'NONE',  ( 9.095951983579540823, -0.8728861028336062367, 41.83160227757072391 ) ) ;
#6885 = CARTESIAN_POINT ( 'NONE',  ( 7.995545880304246289, 59.98659813632740878, -32.45264704635820152 ) ) ;
#6886 = DIRECTION ( 'NONE',  ( 0.000000000000000000, 0.000000000000000000, 1.000000000000000000 ) ) ;
#6887 = PRESENTATION_STYLE_ASSIGNMENT (( #8484 ) ) ;
#6888 = CARTESIAN_POINT ( 'NONE',  ( -23.54759692749571087, 59.99999999999999289, 18.58791755254458877 ) ) ;
#6889 = ORIENTED_EDGE ( 'NONE', *, *, #7554, .T. ) ;
#6890 = DIRECTION ( 'NONE',  ( 0.000000000000000000, 0.000000000000000000, 1.000000000000000000 ) ) ;
#6891 = DIRECTION ( 'NONE',  ( 1.820952055660014662E-28, 1.000000000000000000, -6.508102468073347395E-30 ) ) ;
#6892 = VERTEX_POINT ( 'NONE', #2614 ) ;
#6893 = LINE ( 'NONE', #53, #5422 ) ;
#6894 = CARTESIAN_POINT ( 'NONE',  ( 37.52916669695763119, 61.87792984901915361, 4.938418073206593206 ) ) ;
#6895 = ORIENTED_EDGE ( 'NONE', *, *, #535, .T. ) ;
#6896 = EDGE_CURVE ( 'NONE', #209, #8074, #1835, .T. ) ;
#6897 = EDGE_CURVE ( 'NONE', #7710, #8554, #511, .T. ) ;
#6898 = DIRECTION ( 'NONE',  ( -0.000000000000000000, 1.000000000000000000, -0.000000000000000000 ) ) ;
#6899 =( BOUNDED_SURFACE ( )  B_SPLINE_SURFACE ( 3, 2, ( 
 ( #2281, #29, #9166 ),
 ( #5315, #8418, #8325 ),
 ( #1557, #1647, #3928 ),
 ( #867, #4573, #9119 ),
 ( #4676, #7581, #817 ),
 ( #3825, #82, #6920 ),
 ( #3074, #917, #181 ),
 ( #6092, #2426, #6182 ),
 ( #961, #9213, #5463 ),
 ( #3977, #9352, #8623 ),
 ( #1009, #5653, #9261 ),
 ( #3268, #1845, #4911 ),
 ( #8565, #5509, #322 ),
 ( #4958, #7224, #7775 ),
 ( #2571, #2474, #8664 ),
 ( #4026, #4228, #2669 ),
 ( #9456, #5696, #432 ),
 ( #4076, #8712, #5600 ),
 ( #7066, #1936, #3430 ),
 ( #9411, #1888, #1157 ),
 ( #5552, #3219, #7924 ),
 ( #6429, #7971, #4175 ),
 ( #1106, #7021, #4818 ),
 ( #7829, #6236, #1210 ),
 ( #8518, #1057, #4861 ),
 ( #1747, #282, #4769 ),
 ( #6279, #9306, #2518 ),
 ( #1793, #7121, #3323 ),
 ( #4127, #7879, #6330 ),
 ( #2628, #371, #3372 ),
 ( #7171, #6380, #6577 ),
 ( #8165, #2166, #8857 ),
 ( #6621, #9598, #8956 ),
 ( #614, #5105, #5796 ),
 ( #1396, #1301, #7320 ),
 ( #8112, #5057, #8758 ),
 ( #5883, #661, #2916 ),
 ( #1987, #2869, #2125 ),
 ( #2077, #1349, #8019 ),
 ( #9496, #7268, #4316 ),
 ( #9642, #2819, #520 ),
 ( #570, #3573, #8208 ),
 ( #5010, #4271, #4373 ),
 ( #8904, #7376, #1255 ),
 ( #9692, #4466, #6667 ),
 ( #7425, #3616, #5158 ),
 ( #4413, #3667, #5933 ),
 ( #8807, #3516, #1442 ),
 ( #474, #3470, #2777 ),
 ( #2720, #6523, #5741 ) ),
 .UNSPECIFIED., .F., .F., .F. ) 
 B_SPLINE_SURFACE_WITH_KNOTS ( ( 4, 2, 2, 2, 2, 2, 2, 2, 2, 2, 2, 2, 2, 2, 2, 2, 2, 2, 2, 2, 2, 2, 2, 2, 4 ),
 ( 3, 3 ),
 ( 0.000000000000000000, 0.002954082317436974945, 0.004431123476155462634, 0.005908164634873949890, 0.008862246952310925269, 0.01033928811102941339, 0.01181632926974789978, 0.01329337042846638617, 0.01477041158718487429, 0.01772449390462185054, 0.01920153506334033866, 0.02067857622205882678, 0.02363265853949579956, 0.02510969969821428421, 0.02658674085693277234, 0.02954082317436974858, 0.03249490549180672483, 0.03397194665052521295, 0.03544898780924370107, 0.03840307012668067732, 0.03988011128539916544, 0.04135715244411765357, 0.04431123476155462981, 0.04578827592027311100, 0.04726531707899159912 ),
 ( 0.000000000000000000, 1.000000000000000000 ),
 .UNSPECIFIED. ) 
 GEOMETRIC_REPRESENTATION_ITEM ( )  RATIONAL_B_SPLINE_SURFACE ( (
 ( 1.000000000000000000, 0.7071072458330266430, 1.000000000000000000),
 ( 1.000000000000000000, 0.7071375799977841492, 1.000000000000000000),
 ( 1.000000000000000000, 0.7087768082233868450, 1.000000000000000000),
 ( 1.000000000000000000, 0.7133511096891776981, 1.000000000000000000),
 ( 1.000000000000000000, 0.7152281558699414843, 1.000000000000000000),
 ( 1.000000000000000000, 0.7196307205451061284, 1.000000000000000000),
 ( 1.000000000000000000, 0.7221538050776922235, 1.000000000000000000),
 ( 1.000000000000000000, 0.7303875016897872774, 1.000000000000000000),
 ( 1.000000000000000000, 0.7368055093867738048, 1.000000000000000000),
 ( 1.000000000000000000, 0.7471981614082632284, 1.000000000000000000),
 ( 1.000000000000000000, 0.7508065931793335146, 1.000000000000000000),
 ( 1.000000000000000000, 0.7580362069327493124, 1.000000000000000000),
 ( 1.000000000000000000, 0.7616697343507030649, 1.000000000000000000),
 ( 1.000000000000000000, 0.7688739886174045246, 1.000000000000000000),
 ( 1.000000000000000000, 0.7724449231323486931, 1.000000000000000000),
 ( 1.000000000000000000, 0.7794306818811647108, 1.000000000000000000),
 ( 1.000000000000000000, 0.7828531719709193037, 1.000000000000000000),
 ( 1.000000000000000000, 0.7926992760373742231, 1.000000000000000000),
 ( 1.000000000000000000, 0.7985472967235329733, 1.000000000000000000),
 ( 1.000000000000000000, 0.8058679620540408761, 1.000000000000000000),
 ( 1.000000000000000000, 0.8080665605449595112, 1.000000000000000000),
 ( 1.000000000000000000, 0.8119141137016852028, 1.000000000000000000),
 ( 1.000000000000000000, 0.8135638752277519758, 1.000000000000000000),
 ( 1.000000000000000000, 0.8175016275210426064, 1.000000000000000000),
 ( 1.000000000000000000, 0.8188321819205268692, 1.000000000000000000),
 ( 1.000000000000000000, 0.8188029246654022764, 1.000000000000000000),
 ( 1.000000000000000000, 0.8184514831026776793, 1.000000000000000000),
 ( 1.000000000000000000, 0.8170668779174434793, 1.000000000000000000),
 ( 1.000000000000000000, 0.8160425189860588402, 1.000000000000000000),
 ( 1.000000000000000000, 0.8120414287524539976, 1.000000000000000000),
 ( 1.000000000000000000, 0.8081376665146275950, 1.000000000000000000),
 ( 1.000000000000000000, 0.7981628223982122350, 1.000000000000000000),
 ( 1.000000000000000000, 0.7922386866413546613, 1.000000000000000000),
 ( 1.000000000000000000, 0.7824610464937379328, 1.000000000000000000),
 ( 1.000000000000000000, 0.7790505716245198498, 1.000000000000000000),
 ( 1.000000000000000000, 0.7720072585628966477, 1.000000000000000000),
 ( 1.000000000000000000, 0.7683746194114399186, 1.000000000000000000),
 ( 1.000000000000000000, 0.7575115753154673115, 1.000000000000000000),
 ( 1.000000000000000000, 0.7502382420823103804, 1.000000000000000000),
 ( 1.000000000000000000, 0.7398999340212725206, 1.000000000000000000),
 ( 1.000000000000000000, 0.7365339334704935625, 1.000000000000000000),
 ( 1.000000000000000000, 0.7301925391221738559, 1.000000000000000000),
 ( 1.000000000000000000, 0.7272302897292030055, 1.000000000000000000),
 ( 1.000000000000000000, 0.7191033356628879769, 1.000000000000000000),
 ( 1.000000000000000000, 0.7146970297638910452, 1.000000000000000000),
 ( 1.000000000000000000, 0.7101546834031202682, 1.000000000000000000),
 ( 1.000000000000000000, 0.7089943425723855830, 1.000000000000000000),
 ( 1.000000000000000000, 0.7074683247141949627, 1.000000000000000000),
 ( 1.000000000000000000, 0.7070924731818782893, 1.000000000000000000),
 ( 1.000000000000000000, 0.7071071909622612672, 1.000000000000000000) ) ) 
 REPRESENTATION_ITEM ( '' )  SURFACE ( )  );
#6900 = EDGE_CURVE ( 'NONE', #3082, #8311, #6416, .T. ) ;
#6901 = ADVANCED_BREP_SHAPE_REPRESENTATION ( '', ( #9444, #6314 ), #3968 ) ;
#6902 = CARTESIAN_POINT ( 'NONE',  ( 28.33333333333337833, 59.99999999999999289, -9.860132971832594961 ) ) ;
#6903 = ORIENTED_EDGE ( 'NONE', *, *, #7366, .T. ) ;
#6904 = CARTESIAN_POINT ( 'NONE',  ( 2.581953869975504023, -6.371684584926125439, 43.83179311693056945 ) ) ;
#6905 = CONTEXT_DEPENDENT_SHAPE_REPRESENTATION ( #3213, #87 ) ;
#6906 = ORIENTED_EDGE ( 'NONE', *, *, #1550, .T. ) ;
#6907 = CARTESIAN_POINT ( 'NONE',  ( 0.000000000000000000, 30.00000000000000000, 30.00000000000000711 ) ) ;
#6908 = DIRECTION ( 'NONE',  ( 0.000000000000000000, 0.000000000000000000, 1.000000000000000000 ) ) ;
#6909 = ORIENTED_EDGE ( 'NONE', *, *, #6001, .T. ) ;
#6910 = DIRECTION ( 'NONE',  ( -1.735493991486225972E-29, 6.508102468073347395E-30, 1.000000000000000000 ) ) ;
#6911 = ORIENTED_EDGE ( 'NONE', *, *, #3845, .F. ) ;
#6912 = ADVANCED_FACE ( 'NONE', ( #1094 ), #9392, .F. ) ;
#6913 = EDGE_CURVE ( 'NONE', #8258, #6796, #360, .T. ) ;
#6914 = DIRECTION ( 'NONE',  ( 0.000000000000000000, 1.000000000000000000, 0.000000000000000000 ) ) ;
#6915 = CARTESIAN_POINT ( 'NONE',  ( -5.055427336041082853, -5.357477219937782031, 43.34939598124812221 ) ) ;
#6916 = ORIENTED_EDGE ( 'NONE', *, *, #3845, .T. ) ;
#6917 = FACE_OUTER_BOUND ( 'NONE', #8801, .T. ) ;
#6918 = VERTEX_POINT ( 'NONE', #8508 ) ;
#6919 = EDGE_LOOP ( 'NONE', ( #907, #6228, #564, #5198 ) ) ;
#6920 = CARTESIAN_POINT ( 'NONE',  ( -3.252605054599032819, -6.167148258234369074, 43.73125209769538202 ) ) ;
#6921 =( NAMED_UNIT ( * ) SI_UNIT ( $, .STERADIAN. ) SOLID_ANGLE_UNIT ( ) );
#6922 = CARTESIAN_POINT ( 'NONE',  ( 38.00000000000000711, 39.99999999999999289, 1.326762908760390927E-13 ) ) ;
#6923 = VECTOR ( 'NONE', #6752, 1000.000000000000000 ) ;
#6924 = CONICAL_SURFACE ( 'NONE', #2187, 17.99999999999999645, 0.7853981633974447263 ) ;
#6925 = EDGE_CURVE ( 'NONE', #8659, #928, #1758, .T. ) ;
#6926 = ORIENTED_EDGE ( 'NONE', *, *, #574, .T. ) ;
#6927 = CARTESIAN_POINT ( 'NONE',  ( -33.06426808735054124, 60.99999999999999289, -5.562309845534586294 ) ) ;
#6928 = CARTESIAN_POINT ( 'NONE',  ( 1.300000000000000044, -1.443375672974064328, -9.326206579303807412E-18 ) ) ;
#6929 = EDGE_LOOP ( 'NONE', ( #3924, #8406, #6020, #6926, #9729, #6078, #1829, #8298, #1581, #6193, #798, #3866, #706, #3005, #408, #9546, #6875, #4170, #7531, #3042, #2385, #8461, #5099, #7108, #8764, #2218, #5582, #7382, #4363, #7277, #729, #4660, #7369, #698, #3880, #6086, #6572, #111, #4963, #501, #369, #321, #7303, #9063, #5371, #5547, #6983, #4980, #1844, #4742, #781, #1895 ) ) ;
#6930 = CARTESIAN_POINT ( 'NONE',  ( 0.000000000000000000, 59.99999999999999289, 0.000000000000000000 ) ) ;
#6931 = CARTESIAN_POINT ( 'NONE',  ( 7.989536001449266678, 59.73029374780621481, -33.69619452719668118 ) ) ;
#6932 = PLANE ( 'NONE',  #3495 ) ;
#6933 = CARTESIAN_POINT ( 'NONE',  ( 4.442985217580348589, 17.45059719192358116, 38.75089293311010863 ) ) ;
#6934 = CARTESIAN_POINT ( 'NONE',  ( 2.568784777805632302, 60.99999999999999289, 16.29881421347313974 ) ) ;
#6935 = ORIENTED_EDGE ( 'NONE', *, *, #6063, .T. ) ;
#6936 = TOROIDAL_SURFACE ( 'NONE', #8206, 2.199999999999999734, 0.2000000000000000111 ) ;
#6937 = CARTESIAN_POINT ( 'NONE',  ( -31.00000000000001066, 27.95223080783002345, 1.991564994335481398 ) ) ;
#6938 = CIRCLE ( 'NONE', #5220, 37.99999999999999289 ) ;
#6939 = DIRECTION ( 'NONE',  ( 0.3286710990611016459, -0.000000000000000000, 0.9444444444444404230 ) ) ;
#6940 = ORIENTED_EDGE ( 'NONE', *, *, #8292, .T. ) ;
#6941 = DIRECTION ( 'NONE',  ( -0.000000000000000000, 1.000000000000000000, -0.000000000000000000 ) ) ;
#6942 = CARTESIAN_POINT ( 'NONE',  ( 37.42097066196858179, 61.92370482830305889, 4.403127714044224206 ) ) ;
#6943 = ORIENTED_EDGE ( 'NONE', *, *, #4021, .T. ) ;
#6944 = EDGE_CURVE ( 'NONE', #849, #7361, #9023, .T. ) ;
#6945 = CYLINDRICAL_SURFACE ( 'NONE', #7131, 25.00000000000000000 ) ;
#6946 = CARTESIAN_POINT ( 'NONE',  ( 0.000000000000000000, 39.99999999999999289, 0.000000000000000000 ) ) ;
#6947 = EDGE_LOOP ( 'NONE', ( #1156, #4824, #5434, #1155, #8997, #6317 ) ) ;
#6948 = EDGE_CURVE ( 'NONE', #9587, #987, #4806, .T. ) ;
#6949 = CARTESIAN_POINT ( 'NONE',  ( 1.021055725781022764E-26, 56.00000000000030553, 3.016006292910411346E-28 ) ) ;
#6950 = DIRECTION ( 'NONE',  ( 0.000000000000000000, 0.000000000000000000, -1.000000000000000000 ) ) ;
#6951 = EDGE_CURVE ( 'NONE', #49, #8403, #7763, .T. ) ;
#6952 = LINE ( 'NONE', #126, #6758 ) ;
#6953 = DIRECTION ( 'NONE',  ( 8.659560562354932858E-17, 0.7071067811865474617, -0.7071067811865474617 ) ) ;
#6954 = CARTESIAN_POINT ( 'NONE',  ( 5.000000000000002665, 30.00000000000000000, -29.00000000000000355 ) ) ;
#6955 = AXIS2_PLACEMENT_3D ( 'NONE', #9129, #6786, #1568 ) ;
#6956 = ORIENTED_EDGE ( 'NONE', *, *, #6531, .T. ) ;
#6957 = DIRECTION ( 'NONE',  ( 0.000000000000000000, 0.000000000000000000, 1.000000000000000000 ) ) ;
#6958 = CARTESIAN_POINT ( 'NONE',  ( -8.976219954598299466, -1.160416084251406632, 41.89115029411580338 ) ) ;
#6959 = CIRCLE ( 'NONE', #2214, 38.00000000000000711 ) ;
#6960 = EDGE_CURVE ( 'NONE', #6149, #9386, #8603, .T. ) ;
#6961 = EDGE_CURVE ( 'NONE', #4074, #996, #9601, .T. ) ;
#6962 = EDGE_LOOP ( 'NONE', ( #5340, #8862, #8754, #4493 ) ) ;
#6963 = CARTESIAN_POINT ( 'NONE',  ( 0.000000000000000000, 39.99999999999999289, -30.00000000000000711 ) ) ;
#6964 = ADVANCED_FACE ( 'NONE', ( #8558 ), #2656, .F. ) ;
#6965 = EDGE_LOOP ( 'NONE', ( #8564, #3918 ) ) ;
#6966 = EDGE_LOOP ( 'NONE', ( #3971, #6365, #3772, #8571 ) ) ;
#6967 = ORIENTED_EDGE ( 'NONE', *, *, #7889, .F. ) ;
#6968 = DIRECTION ( 'NONE',  ( -0.000000000000000000, 1.000000000000000000, 0.000000000000000000 ) ) ;
#6969 = VECTOR ( 'NONE', #5029, 1000.000000000000000 ) ;
#6970 = CARTESIAN_POINT ( 'NONE',  ( 1.555535097482682654E-26, 78.08723716182652197, -25.00000000000000000 ) ) ;
#6971 = CARTESIAN_POINT ( 'NONE',  ( 6.000000000000001776, -10.00000000000000533, -26.32489316217636954 ) ) ;
#6972 = VECTOR ( 'NONE', #6719, 1000.000000000000000 ) ;
#6973 = ORIENTED_EDGE ( 'NONE', *, *, #1707, .F. ) ;
#6974 = CARTESIAN_POINT ( 'NONE',  ( 5.562309845534588959, 59.99999999999999289, -33.06426808735054124 ) ) ;
#6975 = VECTOR ( 'NONE', #4994, 1000.000000000000000 ) ;
#6976 = VERTEX_POINT ( 'NONE', #9342 ) ;
#6977 = LINE ( 'NONE', #9360, #3052 ) ;
#6978 = DIRECTION ( 'NONE',  ( 0.000000000000000000, 0.000000000000000000, 1.000000000000000000 ) ) ;
#6979 = VECTOR ( 'NONE', #9370, 1000.000000000000000 ) ;
#6980 = DIRECTION ( 'NONE',  ( 0.000000000000000000, 1.000000000000000000, 0.000000000000000000 ) ) ;
#6981 =( LENGTH_UNIT ( ) NAMED_UNIT ( * ) SI_UNIT ( .MILLI., .METRE. ) );
#6982 = CARTESIAN_POINT ( 'NONE',  ( -33.06426808735054124, 49.99999999999999289, -3.062309845534580077 ) ) ;
#6983 = ORIENTED_EDGE ( 'NONE', *, *, #9566, .T. ) ;
#6984 = DIRECTION ( 'NONE',  ( -1.820952055660014662E-28, -1.000000000000000000, -7.038118388768679669E-30 ) ) ;
#6985 = CARTESIAN_POINT ( 'NONE',  ( 5.562309845534588959, 49.99999999999999289, -30.56426808735054479 ) ) ;
#6986 = DIRECTION ( 'NONE',  ( 0.000000000000000000, 0.000000000000000000, 1.000000000000000000 ) ) ;
#6987 = VERTEX_POINT ( 'NONE', #4452 ) ;
#6988 = CARTESIAN_POINT ( 'NONE',  ( -10.79742499427301894, 59.99999999999999289, 31.18357922838635332 ) ) ;
#6989 = CARTESIAN_POINT ( 'NONE',  ( 5.000000000000009770, 30.00000000000000000, 30.00000000000000711 ) ) ;
#6990 = ORIENTED_EDGE ( 'NONE', *, *, #2601, .T. ) ;
#6991 = VECTOR ( 'NONE', #4324, 1000.000000000000227 ) ;
#6992 = LINE ( 'NONE', #259, #4302 ) ;
#6993 = CIRCLE ( 'NONE', #6371, 27.00000000000000355 ) ;
#6994 = VECTOR ( 'NONE', #448, 1000.000000000000114 ) ;
#6995 = DIRECTION ( 'NONE',  ( -0.000000000000000000, -1.000000000000000000, -0.000000000000000000 ) ) ;
#6996 = VERTEX_POINT ( 'NONE', #3503 ) ;
#6997 = DIRECTION ( 'NONE',  ( -0.000000000000000000, 1.000000000000000000, -0.000000000000000000 ) ) ;
#6998 = LINE ( 'NONE', #265, #7352 ) ;
#6999 = VECTOR ( 'NONE', #9470, 1000.000000000000000 ) ;
#7000 = EDGE_LOOP ( 'NONE', ( #5820, #1819, #1800, #7868 ) ) ;
#7001 = CARTESIAN_POINT ( 'NONE',  ( 30.00000000000000711, 39.99999999999999289, 1.047444401652940259E-13 ) ) ;
#7002 = ORIENTED_EDGE ( 'NONE', *, *, #6292, .T. ) ;
#7003 = DIRECTION ( 'NONE',  ( -0.000000000000000000, 1.000000000000000000, -0.000000000000000000 ) ) ;
#7004 = VERTEX_POINT ( 'NONE', #8747 ) ;
#7005 = EDGE_CURVE ( 'NONE', #2376, #4857, #3659, .T. ) ;
#7006 = DIRECTION ( 'NONE',  ( -0.000000000000000000, -0.000000000000000000, 1.000000000000000000 ) ) ;
#7007 = EDGE_CURVE ( 'NONE', #8330, #8986, #6514, .T. ) ;
#7008 = CYLINDRICAL_SURFACE ( 'NONE', #2124, 25.00000000000000000 ) ;
#7009 = AXIS2_PLACEMENT_3D ( 'NONE', #1344, #4369, #8062 ) ;
#7010 = CIRCLE ( 'NONE', #9712, 38.00000000000000711 ) ;
#7011 = VERTEX_POINT ( 'NONE', #6566 ) ;
#7012 = CARTESIAN_POINT ( 'NONE',  ( -35.42756555166880617, 59.00049740791308039, -6.394654627632702315 ) ) ;
#7013 = AXIS2_PLACEMENT_3D ( 'NONE', #1197, #6321, #7814 ) ;
#7014 = VERTEX_POINT ( 'NONE', #5827 ) ;
#7015 = ORIENTED_EDGE ( 'NONE', *, *, #8714, .F. ) ;
#7016 = CYLINDRICAL_SURFACE ( 'NONE', #9084, 27.99999999999999289 ) ;
#7017 = ORIENTED_EDGE ( 'NONE', *, *, #337, .T. ) ;
#7018 = ORIENTED_EDGE ( 'NONE', *, *, #4639, .T. ) ;
#7019 = AXIS2_PLACEMENT_3D ( 'NONE', #8331, #1369, #4390 ) ;
#7020 = VECTOR ( 'NONE', #6082, 1000.000000000000000 ) ;
#7021 = CARTESIAN_POINT ( 'NONE',  ( -9.682304602691038653, 0.7514046476754797643, 37.93829281883135707 ) ) ;
#7022 = EDGE_CURVE ( 'NONE', #517, #185, #8050, .T. ) ;
#7023 = EDGE_CURVE ( 'NONE', #9740, #6423, #9630, .T. ) ;
#7024 = FACE_OUTER_BOUND ( 'NONE', #7970, .T. ) ;
#7025 = EDGE_CURVE ( 'NONE', #7275, #209, #9588, .T. ) ;
#7026 = DIRECTION ( 'NONE',  ( -0.000000000000000000, 1.000000000000000000, -0.000000000000000000 ) ) ;
#7027 = ORIENTED_EDGE ( 'NONE', *, *, #8430, .F. ) ;
#7028 = CARTESIAN_POINT ( 'NONE',  ( 0.000000000000000000, 3.294852476641296768, 295.0000000000000000 ) ) ;
#7029 = CARTESIAN_POINT ( 'NONE',  ( -3.265277612493196369, 59.85134567364465141, 34.06652594440189574 ) ) ;
#7030 = VERTEX_POINT ( 'NONE', #3557 ) ;
#7031 = FACE_OUTER_BOUND ( 'NONE', #7315, .T. ) ;
#7032 = CARTESIAN_POINT ( 'NONE',  ( 5.206952648169308695, 59.04364549838359721, -35.56426808735298550 ) ) ;
#7033 = VECTOR ( 'NONE', #1638, 1000.000000000000000 ) ;
#7034 = CARTESIAN_POINT ( 'NONE',  ( 0.000000000000000000, 39.99999999999999289, -38.00000000000000711 ) ) ;
#7035 = LINE ( 'NONE', #3895, #4914 ) ;
#7036 = ADVANCED_FACE ( 'NONE', ( #2806 ), #7459, .T. ) ;
#7037 = CARTESIAN_POINT ( 'NONE',  ( 0.000000000000000000, 60.99999999999999289, 0.000000000000000000 ) ) ;
#7038 = EDGE_CURVE ( 'NONE', #1527, #6748, #7410, .T. ) ;
#7039 = FACE_OUTER_BOUND ( 'NONE', #6243, .T. ) ;
#7040 = ORIENTED_EDGE ( 'NONE', *, *, #396, .F. ) ;
#7041 = CARTESIAN_POINT ( 'NONE',  ( 0.000000000000000000, -10.00000000000000533, 0.000000000000000000 ) ) ;
#7042 = DIRECTION ( 'NONE',  ( -1.000000000000000000, -0.000000000000000000, -0.000000000000000000 ) ) ;
#7043 = ORIENTED_EDGE ( 'NONE', *, *, #2924, .F. ) ;
#7044 = CARTESIAN_POINT ( 'NONE',  ( 0.01843853345419280837, 13.29483547765106799, 43.99999130734108377 ) ) ;
#7045 = DIRECTION ( 'NONE',  ( -1.000000000000000000, 0.000000000000000000, 2.168404344971006649E-16 ) ) ;
#7046 = CARTESIAN_POINT ( 'NONE',  ( -36.86535760663189620, 61.99999999999999289, -3.153634179030289530 ) ) ;
#7047 = CARTESIAN_POINT ( 'NONE',  ( 0.000000000000000000, 39.99999999999999289, 19.00000000000005684 ) ) ;
#7048 = LINE ( 'NONE', #1827, #8933 ) ;
#7049 = EDGE_CURVE ( 'NONE', #3249, #7994, #9190, .T. ) ;
#7050 = EDGE_LOOP ( 'NONE', ( #1215, #6258 ) ) ;
#7051 = CARTESIAN_POINT ( 'NONE',  ( 15.97678174684330799, 60.99999999999999289, -28.87459861216662205 ) ) ;
#7052 = VERTEX_POINT ( 'NONE', #9675 ) ;
#7053 = CARTESIAN_POINT ( 'NONE',  ( -28.33333333333344939, 59.99999999999999289, 9.860132971832396009 ) ) ;
#7054 = ORIENTED_EDGE ( 'NONE', *, *, #3833, .T. ) ;
#7055 = EDGE_CURVE ( 'NONE', #4857, #3235, #6959, .T. ) ;
#7056 = CARTESIAN_POINT ( 'NONE',  ( -5.562309845534584518, 49.99999999999999289, 33.06426808735054124 ) ) ;
#7057 = CARTESIAN_POINT ( 'NONE',  ( -5.562309845534584518, 49.99999999999999289, 33.06426808735054124 ) ) ;
#7058 = CARTESIAN_POINT ( 'NONE',  ( -8.545448575588396878, -1.822314913379202564E-27, -24.55555555555564951 ) ) ;
#7059 = VERTEX_POINT ( 'NONE', #8797 ) ;
#7060 = FACE_OUTER_BOUND ( 'NONE', #9677, .T. ) ;
#7061 = EDGE_LOOP ( 'NONE', ( #4804, #6990, #7827, #7783 ) ) ;
#7062 = EDGE_LOOP ( 'NONE', ( #8158, #2022, #2896, #5493 ) ) ;
#7063 = CARTESIAN_POINT ( 'NONE',  ( 34.57348461147494589, 59.39325349372419538, 7.561715963717769107 ) ) ;
#7064 = ORIENTED_EDGE ( 'NONE', *, *, #5282, .F. ) ;
#7065 = ORIENTED_EDGE ( 'NONE', *, *, #9384, .F. ) ;
#7066 = CARTESIAN_POINT ( 'NONE',  ( -11.95253140555284510, -3.346676843148376435, 37.12490603789503041 ) ) ;
#7067 = FACE_OUTER_BOUND ( 'NONE', #2462, .T. ) ;
#7068 = ADVANCED_FACE ( 'NONE', ( #5090 ), #2854, .T. ) ;
#7069 = DIRECTION ( 'NONE',  ( 0.000000000000000000, 0.000000000000000000, 1.000000000000000000 ) ) ;
#7070 = AXIS2_PLACEMENT_3D ( 'NONE', #9652, #7931, #441 ) ;
#7071 = VERTEX_POINT ( 'NONE', #2899 ) ;
#7072 = FACE_OUTER_BOUND ( 'NONE', #7488, .T. ) ;
#7073 = ORIENTED_EDGE ( 'NONE', *, *, #9698, .T. ) ;
#7074 = ORIENTED_EDGE ( 'NONE', *, *, #7337, .F. ) ;
#7075 = CARTESIAN_POINT ( 'NONE',  ( -24.67792535850613334, 30.00000000000000000, -3.999999999999997335 ) ) ;
#7076 = EDGE_CURVE ( 'NONE', #8562, #2569, #5917, .T. ) ;
#7077 = DIRECTION ( 'NONE',  ( 0.000000000000000000, 1.000000000000000000, 0.000000000000000000 ) ) ;
#7078 = CARTESIAN_POINT ( 'NONE',  ( 2.204364238465235033E-15, 38.99999999999993605, -17.99999999999999645 ) ) ;
#7079 = DIRECTION ( 'NONE',  ( 0.000000000000000000, 0.000000000000000000, 1.000000000000000000 ) ) ;
#7080 = CARTESIAN_POINT ( 'NONE',  ( -30.18708036726492594, 60.99999999999999289, -16.70299909897287094 ) ) ;
#7081 = EDGE_CURVE ( 'NONE', #4910, #7266, #7283, .T. ) ;
#7082 = CARTESIAN_POINT ( 'NONE',  ( 11.80999999999999872, 2.449293598294706414E-16, -2.000000000000000000 ) ) ;
#7083 = CIRCLE ( 'NONE', #1573, 5.000000000000000888 ) ;
#7084 = CIRCLE ( 'NONE', #8360, 4.999999999999997335 ) ;
#7085 = VECTOR ( 'NONE', #7497, 1000.000000000000000 ) ;
#7086 = EDGE_CURVE ( 'NONE', #4852, #8258, #6605, .T. ) ;
#7087 = EDGE_CURVE ( 'NONE', #3981, #1595, #4255, .T. ) ;
#7088 = ORIENTED_EDGE ( 'NONE', *, *, #8815, .F. ) ;
#7089 = CARTESIAN_POINT ( 'NONE',  ( 25.51470164434615029, 30.00000000000000000, -5.000000000000007105 ) ) ;
#7090 = VECTOR ( 'NONE', #304, 1000.000000000000000 ) ;
#7091 = CARTESIAN_POINT ( 'NONE',  ( 7.285056225244056734E-27, 40.00000000000013500, 2.827265158360462232E-28 ) ) ;
#7092 = PRODUCT_DEFINITION_SHAPE ( 'NONE', 'NONE',  #4948 ) ;
#7093 = EDGE_CURVE ( 'NONE', #3873, #4022, #5143, .T. ) ;
#7094 = EDGE_LOOP ( 'NONE', ( #5468, #3331, #6732, #8216 ) ) ;
#7095 = DIRECTION ( 'NONE',  ( -0.000000000000000000, 1.000000000000000000, -0.000000000000000000 ) ) ;
#7096 = CARTESIAN_POINT ( 'NONE',  ( -6.000000000000005329, 30.00000000000000000, -26.32489316217636954 ) ) ;
#7097 = ORIENTED_EDGE ( 'NONE', *, *, #8267, .F. ) ;
#7098 = LINE ( 'NONE', #1961, #3535 ) ;
#7099 = DIRECTION ( 'NONE',  ( 0.000000000000000000, -0.000000000000000000, 1.000000000000000000 ) ) ;
#7100 = VECTOR ( 'NONE', #7336, 1000.000000000000227 ) ;
#7101 = CARTESIAN_POINT ( 'NONE',  ( -36.80315167070719440, 61.92350945662830952, -8.081333402833552171 ) ) ;
#7102 = CARTESIAN_POINT ( 'NONE',  ( 2.177727725415564031, -6.478184457066049617, 38.96022561987926025 ) ) ;
#7103 = CARTESIAN_POINT ( 'NONE',  ( 1.300000000000000044, 0.7216878364870328300, 1.250000000000000000 ) ) ;
#7104 =( GEOMETRIC_REPRESENTATION_CONTEXT ( 3 ) GLOBAL_UNCERTAINTY_ASSIGNED_CONTEXT ( ( #9010 ) ) GLOBAL_UNIT_ASSIGNED_CONTEXT ( ( #6981, #5563, #1022 ) ) REPRESENTATION_CONTEXT ( 'NONE', 'WORKASPACE' ) );
#7105 = VERTEX_POINT ( 'NONE', #9485 ) ;
#7106 = DIRECTION ( 'NONE',  ( 0.000000000000000000, 0.000000000000000000, 1.000000000000000000 ) ) ;
#7107 = CARTESIAN_POINT ( 'NONE',  ( 6.000000000000007994, 27.42469319230600533, 31.00000000000000711 ) ) ;
#7108 = ORIENTED_EDGE ( 'NONE', *, *, #8910, .T. ) ;
#7109 = CARTESIAN_POINT ( 'NONE',  ( 33.06426808735054124, 69.99999999999998579, 5.562309845534586294 ) ) ;
#7110 = CARTESIAN_POINT ( 'NONE',  ( 0.000000000000000000, 39.99999999999999289, -40.00000000000000711 ) ) ;
#7111 = AXIS2_PLACEMENT_3D ( 'NONE', #3739, #6734, #9076 ) ;
#7112 = DIRECTION ( 'NONE',  ( 0.000000000000000000, 0.000000000000000000, 1.000000000000000000 ) ) ;
#7113 = VERTEX_POINT ( 'NONE', #5731 ) ;
#7114 = VERTEX_POINT ( 'NONE', #7257 ) ;
#7115 = CARTESIAN_POINT ( 'NONE',  ( 0.000000000000000000, 59.99999999999999289, 0.000000000000000000 ) ) ;
#7116 = ORIENTED_EDGE ( 'NONE', *, *, #7201, .F. ) ;
#7117 = EDGE_LOOP ( 'NONE', ( #9682, #5823, #180, #4480 ) ) ;
#7118 = LINE ( 'NONE', #4816, #4353 ) ;
#7119 = ORIENTED_EDGE ( 'NONE', *, *, #6186, .F. ) ;
#7120 = VERTEX_POINT ( 'NONE', #505 ) ;
#7121 = CARTESIAN_POINT ( 'NONE',  ( -9.894639143346440235, 4.799117292280135061, 37.88549633979417308 ) ) ;
#7122 = DIRECTION ( 'NONE',  ( 0.1178511301977574338, 0.7071067811865470176, 0.6972166887783970424 ) ) ;
#7123 = AXIS2_PLACEMENT_3D ( 'NONE', #7056, #1048, #3457 ) ;
#7124 = DIRECTION ( 'NONE',  ( -1.000000000000000000, 0.000000000000000000, 0.000000000000000000 ) ) ;
#7125 = ORIENTED_EDGE ( 'NONE', *, *, #3169, .T. ) ;
#7126 = ORIENTED_EDGE ( 'NONE', *, *, #5350, .T. ) ;
#7127 = CARTESIAN_POINT ( 'NONE',  ( 1.555535097482682654E-26, 78.08723716182652197, -25.00000000000000000 ) ) ;
#7128 = ORIENTED_EDGE ( 'NONE', *, *, #9110, .T. ) ;
#7129 = EDGE_CURVE ( 'NONE', #9400, #5230, #4926, .T. ) ;
#7130 = DIRECTION ( 'NONE',  ( -0.000000000000000000, -1.000000000000000000, -0.000000000000000000 ) ) ;
#7131 = AXIS2_PLACEMENT_3D ( 'NONE', #207, #6207, #7748 ) ;
#7132 = DIRECTION ( 'NONE',  ( -0.000000000000000000, 1.000000000000000000, -0.000000000000000000 ) ) ;
#7133 = DIRECTION ( 'NONE',  ( 0.000000000000000000, 0.000000000000000000, 1.000000000000000000 ) ) ;
#7134 = CARTESIAN_POINT ( 'NONE',  ( 11.07761026121386294, -5.000000000000018652, 37.39366993089406321 ) ) ;
#7135 = CARTESIAN_POINT ( 'NONE',  ( 35.90836395996004171, 54.99999999999999289, 12.43339847825378186 ) ) ;
#7136 = CARTESIAN_POINT ( 'NONE',  ( -30.12488991936162108, 28.28385863652523824, 6.000000000000009770 ) ) ;
#7137 = CIRCLE ( 'NONE', #4473, 4.324969328314201888 ) ;
#7138 = DIRECTION ( 'NONE',  ( 0.000000000000000000, 0.000000000000000000, 1.000000000000000000 ) ) ;
#7139 = ORIENTED_EDGE ( 'NONE', *, *, #2601, .F. ) ;
#7140 = CARTESIAN_POINT ( 'NONE',  ( 7.307810609882085195, 10.12862448845246277, 42.61414511801761051 ) ) ;
#7141 = VERTEX_POINT ( 'NONE', #4651 ) ;
#7142 = CARTESIAN_POINT ( 'NONE',  ( 0.000000000000000000, 30.00000000000000000, 0.000000000000000000 ) ) ;
#7143 = DIRECTION ( 'NONE',  ( -1.820952055660014662E-28, -1.000000000000000000, 6.508102468073347395E-30 ) ) ;
#7144 = EDGE_LOOP ( 'NONE', ( #9052, #4060, #2452, #1712, #1013 ) ) ;
#7145 = CARTESIAN_POINT ( 'NONE',  ( -12.92730786270479371, 6.859753899161747270, 36.79536516033844151 ) ) ;
#7146 = EDGE_CURVE ( 'NONE', #7876, #6976, #1681, .T. ) ;
#7147 = EDGE_CURVE ( 'NONE', #2169, #3433, #9340, .T. ) ;
#7148 = LINE ( 'NONE', #8693, #3348 ) ;
#7149 = EDGE_CURVE ( 'NONE', #3981, #8583, #5388, .T. ) ;
#7150 = ADVANCED_FACE ( 'NONE', ( #7608 ), #7705, .F. ) ;
#7151 = CARTESIAN_POINT ( 'NONE',  ( 30.18708036726505028, 61.99999999999999289, 16.70299909897265778 ) ) ;
#7152 = FACE_OUTER_BOUND ( 'NONE', #9089, .T. ) ;
#7153 = DIRECTION ( 'NONE',  ( -1.820952055660014662E-28, -1.000000000000000000, -7.038118388768679669E-30 ) ) ;
#7154 = VERTEX_POINT ( 'NONE', #9191 ) ;
#7155 = CARTESIAN_POINT ( 'NONE',  ( 9.219811829770575476E-27, 50.50000000000031974, -26.00000000000008171 ) ) ;
#7156 = ORIENTED_EDGE ( 'NONE', *, *, #3712, .T. ) ;
#7157 = CARTESIAN_POINT ( 'NONE',  ( -31.16666666666624863, 54.99999999999999289, 10.84614626901719170 ) ) ;
#7158 = ORIENTED_EDGE ( 'NONE', *, *, #5619, .F. ) ;
#7159 = CIRCLE ( 'NONE', #8110, 29.00000000000001776 ) ;
#7160 = FACE_OUTER_BOUND ( 'NONE', #354, .T. ) ;
#7161 = CARTESIAN_POINT ( 'NONE',  ( -26.32489316217636954, -15.00000000000000000, -5.999999999999995559 ) ) ;
#7162 = PRODUCT_DEFINITION_CONTEXT ( 'detailed design', #3733, 'design' ) ;
#7163 =( LENGTH_UNIT ( ) NAMED_UNIT ( * ) SI_UNIT ( .MILLI., .METRE. ) );
#7164 = AXIS2_PLACEMENT_3D ( 'NONE', #7450, #6795, #3747 ) ;
#7165 = CARTESIAN_POINT ( 'NONE',  ( 33.06426808735054124, 49.99999999999999289, 5.562309845534586294 ) ) ;
#7166 = ORIENTED_EDGE ( 'NONE', *, *, #5874, .F. ) ;
#7167 = CARTESIAN_POINT ( 'NONE',  ( 33.06426808735054124, 59.99999999999999289, 8.062309845534588959 ) ) ;
#7168 = VERTEX_POINT ( 'NONE', #847 ) ;
#7169 = CARTESIAN_POINT ( 'NONE',  ( -24.67792535850613334, 30.00000000000000000, 4.000000000000009770 ) ) ;
#7170 = ORIENTED_EDGE ( 'NONE', *, *, #9460, .F. ) ;
#7171 = CARTESIAN_POINT ( 'NONE',  ( -12.60343472940743759, 8.172595550171486423, 36.90908749395671862 ) ) ;
#7172 = CIRCLE ( 'NONE', #7654, 38.00000000000000711 ) ;
#7173 = CARTESIAN_POINT ( 'NONE',  ( 1.300000000000000044, -1.443375672974064328, -9.326206579303807412E-18 ) ) ;
#7174 = VECTOR ( 'NONE', #9015, 1000.000000000000000 ) ;
#7175 = CARTESIAN_POINT ( 'NONE',  ( -5.562309845534584518, 69.99999999999998579, 33.06426808735054124 ) ) ;
#7176 = PRODUCT_DEFINITION_SHAPE ( 'NONE', 'NONE',  #9477 ) ;
#7177 = AXIS2_PLACEMENT_3D ( 'NONE', #795, #5286, #8301 ) ;
#7178 = VECTOR ( 'NONE', #8159, 1000.000000000000000 ) ;
#7179 = ORIENTED_EDGE ( 'NONE', *, *, #1609, .T. ) ;
#7180 = DIRECTION ( 'NONE',  ( 0.000000000000000000, 1.000000000000000000, 0.000000000000000000 ) ) ;
#7181 = CIRCLE ( 'NONE', #2127, 17.99999999999999645 ) ;
#7182 = EDGE_CURVE ( 'NONE', #5814, #7014, #6174, .T. ) ;
#7183 = CIRCLE ( 'NONE', #7019, 2.500000000000002220 ) ;
#7184 = ORIENTED_EDGE ( 'NONE', *, *, #8731, .T. ) ;
#7185 = LINE ( 'NONE', #2827, #4566 ) ;
#7186 = DIRECTION ( 'NONE',  ( -0.000000000000000000, 1.000000000000000000, 1.224646799147353207E-16 ) ) ;
#7187 = CARTESIAN_POINT ( 'NONE',  ( 13.15172707401184660, 5.587632569554690676, 36.71574829764672643 ) ) ;
#7188 = CARTESIAN_POINT ( 'NONE',  ( 0.000000000000000000, 0.000000000000000000, 29.00000000000000355 ) ) ;
#7189 = DIRECTION ( 'NONE',  ( -1.820952055660014662E-28, -1.000000000000000000, -7.038118388768679669E-30 ) ) ;
#7190 = VECTOR ( 'NONE', #6575, 1000.000000000000000 ) ;
#7191 = AXIS2_PLACEMENT_3D ( 'NONE', #4848, #4750, #6950 ) ;
#7192 = VECTOR ( 'NONE', #4050, 1000.000000000000000 ) ;
#7193 = ORIENTED_EDGE ( 'NONE', *, *, #635, .F. ) ;
#7194 = DIRECTION ( 'NONE',  ( 0.5773502691896204020, -0.5773502691896365002, -0.5773502691896205130 ) ) ;
#7195 = CARTESIAN_POINT ( 'NONE',  ( 6.127821927972693317, 11.22362876687147626, 43.03694912904850867 ) ) ;
#7196 = ORIENTED_EDGE ( 'NONE', *, *, #5755, .T. ) ;
#7197 = FACE_OUTER_BOUND ( 'NONE', #2852, .T. ) ;
#7198 = PRESENTATION_STYLE_ASSIGNMENT (( #8088 ) ) ;
#7199 = CARTESIAN_POINT ( 'NONE',  ( -10.76024444187491191, 12.20917503714134789, 37.49526129101297300 ) ) ;
#7200 = FACE_OUTER_BOUND ( 'NONE', #7650, .T. ) ;
#7201 = EDGE_CURVE ( 'NONE', #2421, #6620, #8398, .T. ) ;
#7202 = AXIS2_PLACEMENT_3D ( 'NONE', #8137, #8182, #1512 ) ;
#7203 = ORIENTED_EDGE ( 'NONE', *, *, #1246, .F. ) ;
#7204 = DIRECTION ( 'NONE',  ( 0.000000000000000000, -0.000000000000000000, 1.000000000000000000 ) ) ;
#7205 = EDGE_CURVE ( 'NONE', #1252, #2652, #1766, .T. ) ;
#7206 = ORIENTED_EDGE ( 'NONE', *, *, #35, .F. ) ;
#7207 = DIRECTION ( 'NONE',  ( 0.000000000000000000, 0.000000000000000000, 1.000000000000000000 ) ) ;
#7208 = CARTESIAN_POINT ( 'NONE',  ( -4.623603109644814246, -8.639161593214105039, 39.15028058075186124 ) ) ;
#7209 = ADVANCED_FACE ( 'NONE', ( #7656 ), #1582, .F. ) ;
#7210 = ORIENTED_EDGE ( 'NONE', *, *, #5991, .F. ) ;
#7211 = ADVANCED_FACE ( 'NONE', ( #3910 ), #157, .T. ) ;
#7212 = FACE_OUTER_BOUND ( 'NONE', #3965, .T. ) ;
#7213 = CARTESIAN_POINT ( 'NONE',  ( -12.48950176432141923, 59.99999999999999289, -35.88888888888889284 ) ) ;
#7214 = FACE_OUTER_BOUND ( 'NONE', #756, .T. ) ;
#7215 = CARTESIAN_POINT ( 'NONE',  ( 0.000000000000000000, 0.000000000000000000, 0.000000000000000000 ) ) ;
#7216 = ORIENTED_EDGE ( 'NONE', *, *, #6559, .T. ) ;
#7217 = DIRECTION ( 'NONE',  ( -0.1666666666666658525, -3.897465909857536228E-29, -0.9860132971832695770 ) ) ;
#7218 = EDGE_CURVE ( 'NONE', #5104, #1193, #3992, .T. ) ;
#7219 = ORIENTED_EDGE ( 'NONE', *, *, #1001, .F. ) ;
#7220 = CARTESIAN_POINT ( 'NONE',  ( -8.216777476527274970, 47.50000000000033396, -23.61111111111111427 ) ) ;
#7221 = EDGE_LOOP ( 'NONE', ( #3572, #7128, #3904, #8546, #2952 ) ) ;
#7222 = ORIENTED_EDGE ( 'NONE', *, *, #3745, .F. ) ;
#7223 = EDGE_CURVE ( 'NONE', #5938, #8381, #8299, .T. ) ;
#7224 = CARTESIAN_POINT ( 'NONE',  ( -6.823606946495824666, -4.058130453688225892, 38.51596139903070082 ) ) ;
#7225 = EDGE_CURVE ( 'NONE', #3225, #2857, #3752, .T. ) ;
#7226 = CARTESIAN_POINT ( 'NONE',  ( 5.000000000000008882, 30.00000000000000000, 25.51470164434615029 ) ) ;
#7227 = CARTESIAN_POINT ( 'NONE',  ( -24.67792535850613334, 0.000000000000000000, 4.000000000000009770 ) ) ;
#7228 = EDGE_LOOP ( 'NONE', ( #2473, #7679, #2668, #377 ) ) ;
#7229 = CARTESIAN_POINT ( 'NONE',  ( -4.000000000000005329, 30.00000000000000000, 0.000000000000000000 ) ) ;
#7230 = CARTESIAN_POINT ( 'NONE',  ( -3.055999436386194201, 59.99999999999998579, 33.03613408327222345 ) ) ;
#7231 = VERTEX_POINT ( 'NONE', #8447 ) ;
#7232 = LINE ( 'NONE', #3436, #4092 ) ;
#7233 = CARTESIAN_POINT ( 'NONE',  ( 0.000000000000000000, 19.99999999999982236, 0.000000000000000000 ) ) ;
#7234 = CARTESIAN_POINT ( 'NONE',  ( 13.30507877576147280, 2.992956817324265550, 36.66028305328001125 ) ) ;
#7235 = DIRECTION ( 'NONE',  ( 0.000000000000000000, -0.000000000000000000, -1.000000000000000000 ) ) ;
#7236 = CYLINDRICAL_SURFACE ( 'NONE', #7975, 2.500000000000001332 ) ;
#7237 = EDGE_CURVE ( 'NONE', #4569, #5208, #6701, .T. ) ;
#7238 = PLANE ( 'NONE',  #5364 ) ;
#7239 = ORIENTED_EDGE ( 'NONE', *, *, #2116, .F. ) ;
#7240 = CYLINDRICAL_SURFACE ( 'NONE', #3743, 34.49999999999998579 ) ;
#7241 = DIRECTION ( 'NONE',  ( 0.000000000000000000, 0.000000000000000000, 1.000000000000000000 ) ) ;
#7242 = ORIENTED_EDGE ( 'NONE', *, *, #790, .T. ) ;
#7243 = FACE_OUTER_BOUND ( 'NONE', #5472, .T. ) ;
#7244 = DIRECTION ( 'NONE',  ( 0.000000000000000000, 0.000000000000000000, 1.000000000000000000 ) ) ;
#7245 = VECTOR ( 'NONE', #3138, 1000.000000000000000 ) ;
#7246 = CIRCLE ( 'NONE', #477, 38.00000000000000711 ) ;
#7247 = DIRECTION ( 'NONE',  ( -1.000000000000000000, -0.000000000000000000, -3.491481338843134933E-15 ) ) ;
#7248 = CARTESIAN_POINT ( 'NONE',  ( 6.840980308309120517, -7.660779396856534973, 38.68949562317958879 ) ) ;
#7249 = AXIS2_PLACEMENT_3D ( 'NONE', #674, #9659, #1408 ) ;
#7250 = LINE ( 'NONE', #9438, #9379 ) ;
#7251 = ORIENTED_EDGE ( 'NONE', *, *, #6249, .F. ) ;
#7252 = CARTESIAN_POINT ( 'NONE',  ( 0.000000000000000000, 61.99999999999999289, 0.000000000000000000 ) ) ;
#7253 = CARTESIAN_POINT ( 'NONE',  ( -6.343556221692952413, -7.892000900020214260, 38.79899860510401055 ) ) ;
#7254 = EDGE_CURVE ( 'NONE', #7682, #8580, #362, .T. ) ;
#7255 = ORIENTED_EDGE ( 'NONE', *, *, #7022, .F. ) ;
#7256 = AXIS2_PLACEMENT_3D ( 'NONE', #4476, #1998, #8868 ) ;
#7257 = CARTESIAN_POINT ( 'NONE',  ( -15.25056439471426195, 61.99999999999999289, 27.56211685706803038 ) ) ;
#7258 = LINE ( 'NONE', #506, #4043 ) ;
#7259 = EDGE_CURVE ( 'NONE', #5164, #8683, #5411, .T. ) ;
#7260 = ADVANCED_FACE ( 'NONE', ( #1529 ), #2308, .F. ) ;
#7261 = DIRECTION ( 'NONE',  ( 0.000000000000000000, 0.000000000000000000, 1.000000000000000000 ) ) ;
#7262 = CARTESIAN_POINT ( 'NONE',  ( 0.000000000000000000, 0.000000000000000000, 0.000000000000000000 ) ) ;
#7263 = ORIENTED_EDGE ( 'NONE', *, *, #4014, .F. ) ;
#7264 = DIRECTION ( 'NONE',  ( 0.000000000000000000, 0.000000000000000000, 1.000000000000000000 ) ) ;
#7265 = LINE ( 'NONE', #5737, #2918 ) ;
#7266 = VERTEX_POINT ( 'NONE', #3100 ) ;
#7267 = ORIENTED_EDGE ( 'NONE', *, *, #463, .T. ) ;
#7268 = CARTESIAN_POINT ( 'NONE',  ( -4.686466027247337074, 12.16196211887748824, 38.79096271003776053 ) ) ;
#7269 = LINE ( 'NONE', #7321, #4985 ) ;
#7270 = EDGE_CURVE ( 'NONE', #7461, #3950, #5707, .T. ) ;
#7271 = CARTESIAN_POINT ( 'NONE',  ( -5.999999999999998224, 27.42469319230601243, 31.00000000000000711 ) ) ;
#7272 = EDGE_CURVE ( 'NONE', #3069, #5730, #3046, .T. ) ;
#7273 = EDGE_CURVE ( 'NONE', #1089, #2358, #2398, .T. ) ;
#7274 = ADVANCED_FACE ( 'NONE', ( #9436 ), #8498, .T. ) ;
#7275 = VERTEX_POINT ( 'NONE', #397 ) ;
#7276 = CYLINDRICAL_SURFACE ( 'NONE', #8435, 1.500000000000003109 ) ;
#7277 = ORIENTED_EDGE ( 'NONE', *, *, #2248, .T. ) ;
#7278 = ORIENTED_EDGE ( 'NONE', *, *, #3282, .T. ) ;
#7279 = DIRECTION ( 'NONE',  ( -1.820952055660014662E-28, -1.000000000000000000, -7.038118388768679669E-30 ) ) ;
#7280 = DIRECTION ( 'NONE',  ( 0.000000000000000000, 0.000000000000000000, -1.000000000000000000 ) ) ;
#7281 = CYLINDRICAL_SURFACE ( 'NONE', #3164, 10.00000000000001599 ) ;
#7282 = CARTESIAN_POINT ( 'NONE',  ( 8.673617379884035472E-16, 1.899999999999999689, 0.000000000000000000 ) ) ;
#7283 = CIRCLE ( 'NONE', #7926, 5.000000000000000888 ) ;
#7284 = AXIS2_PLACEMENT_3D ( 'NONE', #733, #4435, #883 ) ;
#7285 = DIRECTION ( 'NONE',  ( -1.735493991486225972E-29, 6.508102468073347395E-30, 1.000000000000000000 ) ) ;
#7286 = EDGE_CURVE ( 'NONE', #960, #6115, #5675, .T. ) ;
#7287 = AXIS2_PLACEMENT_3D ( 'NONE', #1630, #1474, #3147 ) ;
#7288 = DIRECTION ( 'NONE',  ( -0.000000000000000000, -1.000000000000000000, -0.000000000000000000 ) ) ;
#7289 = ORIENTED_EDGE ( 'NONE', *, *, #1421, .T. ) ;
#7290 = DIRECTION ( 'NONE',  ( 1.735493991486228214E-29, 0.000000000000000000, -1.000000000000000000 ) ) ;
#7291 = CARTESIAN_POINT ( 'NONE',  ( 9.983264251130078648, 3.962791862995775904, 41.37336488016977398 ) ) ;
#7292 = ORIENTED_EDGE ( 'NONE', *, *, #3562, .F. ) ;
#7293 = DIRECTION ( 'NONE',  ( 0.3286710990610922090, 6.289316826390952918E-29, 0.9444444444444435316 ) ) ;
#7294 = CARTESIAN_POINT ( 'NONE',  ( 9.219811829770575476E-27, 50.50000000000031974, -24.09806918451529612 ) ) ;
#7295 = CARTESIAN_POINT ( 'NONE',  ( 30.00000000000000711, 59.99999999999999289, 1.047444401652940259E-13 ) ) ;
#7296 = VECTOR ( 'NONE', #5885, 1000.000000000000000 ) ;
#7297 = AXIS2_PLACEMENT_3D ( 'NONE', #298, #3247, #203 ) ;
#7298 = CARTESIAN_POINT ( 'NONE',  ( -32.59762842694629370, 60.99999999999999289, 5.137569555611143812 ) ) ;
#7299 = B_SPLINE_CURVE_WITH_KNOTS ( 'NONE', 3,
 ( #2975, #8269, #2220, #9751 ),
 .UNSPECIFIED., .F., .F.,
 ( 4, 4 ),
 ( 0.000000000000000000, 0.003679109433542037191 ),
 .UNSPECIFIED. ) ;
#7300 = AXIS2_PLACEMENT_3D ( 'NONE', #1784, #3363, #5643 ) ;
#7301 = ORIENTED_EDGE ( 'NONE', *, *, #2487, .F. ) ;
#7302 = DIRECTION ( 'NONE',  ( 0.000000000000000000, 0.000000000000000000, -1.000000000000000000 ) ) ;
#7303 = ORIENTED_EDGE ( 'NONE', *, *, #3729, .T. ) ;
#7304 = CARTESIAN_POINT ( 'NONE',  ( -33.06426808735054124, 60.99999999999999289, -5.562309845534586294 ) ) ;
#7305 = CARTESIAN_POINT ( 'NONE',  ( -2.105232674386741554, -14.99999999999968381, 36.76945403167025006 ) ) ;
#7306 = VERTEX_POINT ( 'NONE', #7799 ) ;
#7307 = CARTESIAN_POINT ( 'NONE',  ( 1.203012880462043003E-26, 59.00000000000029843, -25.00000000000000000 ) ) ;
#7308 = DIRECTION ( 'NONE',  ( 0.000000000000000000, 1.000000000000000000, 0.000000000000000000 ) ) ;
#7309 = CARTESIAN_POINT ( 'NONE',  ( 1.148778693228098442E-26, 51.50000000000032685, -37.00000000000000711 ) ) ;
#7310 = DIRECTION ( 'NONE',  ( 0.000000000000000000, -1.000000000000000000, 0.000000000000000000 ) ) ;
#7311 = ORIENTED_EDGE ( 'NONE', *, *, #9031, .F. ) ;
#7312 = DIRECTION ( 'NONE',  ( 0.000000000000000000, 1.000000000000000000, 0.000000000000000000 ) ) ;
#7313 = ORIENTED_EDGE ( 'NONE', *, *, #7761, .T. ) ;
#7314 = CARTESIAN_POINT ( 'NONE',  ( 35.43299232931641995, 59.17741350630852537, 4.746722514775171042 ) ) ;
#7315 = EDGE_LOOP ( 'NONE', ( #5076, #8449, #3318, #6724 ) ) ;
#7316 = CARTESIAN_POINT ( 'NONE',  ( 12.43339847825378364, 59.99999999999999289, -35.90836395996003461 ) ) ;
#7317 = AXIS2_PLACEMENT_3D ( 'NONE', #4096, #340, #3141 ) ;
#7318 =( REPRESENTATION_RELATIONSHIP ('NONE','NONE', #5841, #1483 ) REPRESENTATION_RELATIONSHIP_WITH_TRANSFORMATION ( #1534 )SHAPE_REPRESENTATION_RELATIONSHIP( ) );
#7319 = VERTEX_POINT ( 'NONE', #1866 ) ;
#7320 = CARTESIAN_POINT ( 'NONE',  ( -7.922255980087944849, 9.405859711871766393, 42.36613572011585660 ) ) ;
#7321 = CARTESIAN_POINT ( 'NONE',  ( 23.54759692749571087, 59.99999999999999289, -18.58791755254458167 ) ) ;
#7322 = DIRECTION ( 'NONE',  ( -1.820952055660014662E-28, -1.000000000000000000, -7.038118388768679669E-30 ) ) ;
#7323 = AXIS2_PLACEMENT_3D ( 'NONE', #7037, #293, #838 ) ;
#7324 = VECTOR ( 'NONE', #1377, 1000.000000000000000 ) ;
#7325 = ORIENTED_EDGE ( 'NONE', *, *, #4733, .F. ) ;
#7326 = DIRECTION ( 'NONE',  ( 1.735493991486225972E-29, -6.508102468073347395E-30, -1.000000000000000000 ) ) ;
#7327 = ORIENTED_EDGE ( 'NONE', *, *, #831, .T. ) ;
#7328 = VERTEX_POINT ( 'NONE', #4102 ) ;
#7329 = CARTESIAN_POINT ( 'NONE',  ( -6.000000000000005329, -10.00000000000000533, -31.00000000000000711 ) ) ;
#7330 = EDGE_CURVE ( 'NONE', #137, #4065, #7148, .T. ) ;
#7331 = CIRCLE ( 'NONE', #1033, 26.00000000000009592 ) ;
#7332 = ADVANCED_FACE ( 'NONE', ( #2602 ), #6259, .T. ) ;
#7333 = PLANE ( 'NONE',  #2657 ) ;
#7334 = AXIS2_PLACEMENT_3D ( 'NONE', #8679, #3440, #2737 ) ;
#7335 = FACE_OUTER_BOUND ( 'NONE', #4890, .T. ) ;
#7336 = DIRECTION ( 'NONE',  ( -0.000000000000000000, 0.5000000000000000000, 0.8660254037844385966 ) ) ;
#7337 = EDGE_CURVE ( 'NONE', #8061, #7878, #4938, .T. ) ;
#7338 = CARTESIAN_POINT ( 'NONE',  ( -3.999999999999998224, 28.99999999999997158, 29.00000000000000355 ) ) ;
#7339 = CIRCLE ( 'NONE', #3068, 33.00000000000000711 ) ;
#7340 = AXIS2_PLACEMENT_3D ( 'NONE', #9490, #3566, #2861 ) ;
#7341 = CIRCLE ( 'NONE', #1820, 37.00000000000000711 ) ;
#7342 = AXIS2_PLACEMENT_3D ( 'NONE', #5553, #4960, #2722 ) ;
#7343 = CARTESIAN_POINT ( 'NONE',  ( 4.000000000000007994, 28.99999999999997158, 24.67792535850613334 ) ) ;
#7344 = VERTEX_POINT ( 'NONE', #1083 ) ;
#7345 = PLANE ( 'NONE',  #6723 ) ;
#7346 = DIRECTION ( 'NONE',  ( -0.000000000000000000, -0.5000000000000001110, -0.8660254037844385966 ) ) ;
#7347 = EDGE_CURVE ( 'NONE', #4501, #4883, #4627, .T. ) ;
#7348 = AXIS2_PLACEMENT_3D ( 'NONE', #16, #9108, #5970 ) ;
#7349 = ORIENTED_EDGE ( 'NONE', *, *, #4474, .F. ) ;
#7350 = DIRECTION ( 'NONE',  ( 0.000000000000000000, 0.000000000000000000, 1.000000000000000000 ) ) ;
#7351 = CARTESIAN_POINT ( 'NONE',  ( -31.00000000000000711, 27.42469319230601243, -5.999999999999996447 ) ) ;
#7352 = VECTOR ( 'NONE', #8647, 1000.000000000000000 ) ;
#7353 = ADVANCED_FACE ( 'NONE', ( #9287 ), #3404, .F. ) ;
#7354 = CARTESIAN_POINT ( 'NONE',  ( 2.200000000000000622, 0.000000000000000000, 0.000000000000000000 ) ) ;
#7355 = VECTOR ( 'NONE', #8109, 1000.000000000000000 ) ;
#7356 = ORIENTED_EDGE ( 'NONE', *, *, #4579, .F. ) ;
#7357 = CARTESIAN_POINT ( 'NONE',  ( 0.000000000000000000, 59.99999999999999289, 0.000000000000000000 ) ) ;
#7358 = ORIENTED_EDGE ( 'NONE', *, *, #4998, .T. ) ;
#7359 = DIRECTION ( 'NONE',  ( 0.000000000000000000, 1.000000000000000000, 0.000000000000000000 ) ) ;
#7360 = CARTESIAN_POINT ( 'NONE',  ( -28.87459861216645862, 61.99999999999999289, -15.97678174684361707 ) ) ;
#7361 = VERTEX_POINT ( 'NONE', #4795 ) ;
#7362 = AXIS2_PLACEMENT_3D ( 'NONE', #2557, #2611, #6217 ) ;
#7363 = DIRECTION ( 'NONE',  ( -0.000000000000000000, -1.000000000000000000, -0.000000000000000000 ) ) ;
#7364 = DIRECTION ( 'NONE',  ( 0.000000000000000000, 0.000000000000000000, -1.000000000000000000 ) ) ;
#7365 = ORIENTED_EDGE ( 'NONE', *, *, #4154, .F. ) ;
#7366 = EDGE_CURVE ( 'NONE', #9614, #7306, #8402, .T. ) ;
#7367 = CARTESIAN_POINT ( 'NONE',  ( 6.624374116212009334, 10.81446379339695874, 42.86925100779671993 ) ) ;
#7368 =( NAMED_UNIT ( * ) PLANE_ANGLE_UNIT ( ) SI_UNIT ( $, .RADIAN. ) );
#7369 = ORIENTED_EDGE ( 'NONE', *, *, #2956, .T. ) ;
#7370 = DIRECTION ( 'NONE',  ( -1.000000000000000000, 0.000000000000000000, 2.168404344971006649E-16 ) ) ;
#7371 = ORIENTED_EDGE ( 'NONE', *, *, #2970, .T. ) ;
#7372 = LINE ( 'NONE', #2120, #6058 ) ;
#7373 = EDGE_LOOP ( 'NONE', ( #7946, #8780, #7184, #1285, #8662 ) ) ;
#7374 = FACE_BOUND ( 'NONE', #5660, .T. ) ;
#7375 = ORIENTED_EDGE ( 'NONE', *, *, #834, .T. ) ;
#7376 = CARTESIAN_POINT ( 'NONE',  ( -2.734912810787019311, 12.94483271673466440, 38.93811822664099509 ) ) ;
#7377 = DIRECTION ( 'NONE',  ( -1.735493991486225972E-29, 6.508102468073347395E-30, 1.000000000000000000 ) ) ;
#7378 = FACE_OUTER_BOUND ( 'NONE', #6782, .T. ) ;
#7379 = ORIENTED_EDGE ( 'NONE', *, *, #2924, .T. ) ;
#7380 = DIRECTION ( 'NONE',  ( -0.000000000000000000, -1.000000000000000000, -0.000000000000000000 ) ) ;
#7381 = VERTEX_POINT ( 'NONE', #302 ) ;
#7382 = ORIENTED_EDGE ( 'NONE', *, *, #8849, .T. ) ;
#7383 = LINE ( 'NONE', #531, #5261 ) ;
#7384 = CARTESIAN_POINT ( 'NONE',  ( -35.88888888888889284, 59.99999999999999289, 12.48950176432140857 ) ) ;
#7385 = DIRECTION ( 'NONE',  ( -0.000000000000000000, -0.000000000000000000, 1.000000000000000000 ) ) ;
#7386 = DIRECTION ( 'NONE',  ( -0.000000000000000000, -1.000000000000000000, -0.000000000000000000 ) ) ;
#7387 = EDGE_CURVE ( 'NONE', #6468, #1101, #6013, .T. ) ;
#7388 = DIRECTION ( 'NONE',  ( -1.735493991486225972E-29, 6.508102468073347395E-30, 1.000000000000000000 ) ) ;
#7389 = B_SPLINE_CURVE_WITH_KNOTS ( 'NONE', 3,
 ( #9130, #8429, #4688, #926, #3938, #6933, #193, #3185, #6197, #7985, #6438, #1946, #1901, #536, #6537, #1266, #8676, #484, #9560, #8030, #1221, #5664, #5806, #4237, #8725, #7187, #8077, #7934, #7234, #8772, #3384, #2583, #1315, #9363, #3483, #4872, #4922, #1168, #5615, #7134 ),
 .UNSPECIFIED., .F., .F.,
 ( 4, 2, 2, 2, 2, 2, 2, 2, 2, 2, 2, 2, 2, 2, 2, 2, 2, 2, 2, 4 ),
 ( 0.04534133810020674754, 0.04730715269063350686, 0.04927296728106025925, 0.05123878187148701857, 0.05222168916670039129, 0.05320459646191377096, 0.05517041105234051640, 0.05615331834755388912, 0.05713622564276726185, 0.06106785482362075967, 0.06205076211883412546, 0.06303366941404750512, 0.06499948400447425056, 0.06696529859490098213, 0.06893111318532772758, 0.07089692777575447302, 0.07286274236618120459, 0.07482855695660795003, 0.07581146425182133664, 0.07679437154703469548 ),
 .UNSPECIFIED. ) ;
#7390 = EDGE_CURVE ( 'NONE', #1910, #478, #3198, .T. ) ;
#7391 = CARTESIAN_POINT ( 'NONE',  ( 0.000000000000000000, 1.443375672974065216, 1.084202172492522584E-16 ) ) ;
#7392 = ORIENTED_EDGE ( 'NONE', *, *, #2534, .F. ) ;
#7393 = CARTESIAN_POINT ( 'NONE',  ( -6.235648121649205677, 61.81426382726520075, 37.52627707316312922 ) ) ;
#7394 = CARTESIAN_POINT ( 'NONE',  ( -29.00000000000000355, 30.00000000000000000, -4.999999999999997335 ) ) ;
#7395 = LINE ( 'NONE', #2233, #3399 ) ;
#7396 = CARTESIAN_POINT ( 'NONE',  ( -8.216777476527294510, 44.00000000000019895, -23.61111111111111427 ) ) ;
#7397 = DIRECTION ( 'NONE',  ( -1.820952055660014662E-28, -1.000000000000000000, 6.508102468073347395E-30 ) ) ;
#7398 = B_SPLINE_CURVE_WITH_KNOTS ( 'NONE', 3,
 ( #2891, #8936, #2189, #1422, #7449, #8236, #1465, #4490 ),
 .UNSPECIFIED., .F., .F.,
 ( 4, 2, 2, 4 ),
 ( 8.673617379884035472E-19, 0.006005055813302546432, 0.009007583719953818346, 0.01201011162660509113 ),
 .UNSPECIFIED. ) ;
#7399 = DIRECTION ( 'NONE',  ( 0.000000000000000000, -1.000000000000000000, 0.000000000000000000 ) ) ;
#7400 = B_SPLINE_CURVE_WITH_KNOTS ( 'NONE', 3,
 ( #8941, #8149, #2704, #6601, #1379 ),
 .UNSPECIFIED., .F., .F.,
 ( 4, 1, 4 ),
 ( 0.04531639312264377356, 0.04532886561142526055, 0.04534133810020674754 ),
 .UNSPECIFIED. ) ;
#7401 = ADVANCED_FACE ( 'NONE', ( #3297 ), #6945, .T. ) ;
#7402 = EDGE_CURVE ( 'NONE', #8252, #2652, #6992, .T. ) ;
#7403 = PLANE ( 'NONE',  #2241 ) ;
#7404 = AXIS2_PLACEMENT_3D ( 'NONE', #5259, #7433, #669 ) ;
#7405 = DIRECTION ( 'NONE',  ( -0.000000000000000000, -1.000000000000000000, -0.000000000000000000 ) ) ;
#7406 = VERTEX_POINT ( 'NONE', #8542 ) ;
#7407 = CARTESIAN_POINT ( 'NONE',  ( 0.000000000000000000, 59.99999999999999289, 0.000000000000000000 ) ) ;
#7408 = CARTESIAN_POINT ( 'NONE',  ( 9.488413251914037616, -6.035962460277373154, 37.89468146663847392 ) ) ;
#7409 = ORIENTED_EDGE ( 'NONE', *, *, #5757, .F. ) ;
#7410 = LINE ( 'NONE', #2108, #4295 ) ;
#7411 = CIRCLE ( 'NONE', #8829, 1.500000000000001332 ) ;
#7412 = VECTOR ( 'NONE', #4034, 1000.000000000000000 ) ;
#7413 = FACE_OUTER_BOUND ( 'NONE', #1985, .T. ) ;
#7414 = DIRECTION ( 'NONE',  ( 1.735493991486225972E-29, -6.508102468073347395E-30, -1.000000000000000000 ) ) ;
#7415 = CARTESIAN_POINT ( 'NONE',  ( 12.87078970757343832, 7.181859258121229495, 36.81542066095411059 ) ) ;
#7416 = PRODUCT_CONTEXT ( 'NONE', #7836, 'mechanical' ) ;
#7417 = ORIENTED_EDGE ( 'NONE', *, *, #2687, .T. ) ;
#7418 = CARTESIAN_POINT ( 'NONE',  ( 0.000000000000000000, 59.99999999999999289, 0.000000000000000000 ) ) ;
#7419 = EDGE_LOOP ( 'NONE', ( #4472, #787, #6916, #4402, #170 ) ) ;
#7420 = CARTESIAN_POINT ( 'NONE',  ( 34.92646553026882117, 59.22976218012610161, 7.237999934912880740 ) ) ;
#7421 = EDGE_LOOP ( 'NONE', ( #8839, #3509, #3057, #6625, #286 ) ) ;
#7422 = CARTESIAN_POINT ( 'NONE',  ( -5.562309845534584518, 59.99999999999999289, 30.56426808735054124 ) ) ;
#7423 = AXIS2_PLACEMENT_3D ( 'NONE', #7229, #5700, #479 ) ;
#7424 = ORIENTED_EDGE ( 'NONE', *, *, #710, .T. ) ;
#7425 = CARTESIAN_POINT ( 'NONE',  ( -2.159481158939806189, 18.10398488085508362, 38.94256672920901963 ) ) ;
#7426 = FACE_OUTER_BOUND ( 'NONE', #3792, .T. ) ;
#7427 = CARTESIAN_POINT ( 'NONE',  ( 0.000000000000000000, 39.99999999999999289, -37.99999999999999289 ) ) ;
#7428 = VECTOR ( 'NONE', #3875, 1000.000000000000000 ) ;
#7429 = AXIS2_PLACEMENT_3D ( 'NONE', #1711, #9228, #9180 ) ;
#7430 = ORIENTED_EDGE ( 'NONE', *, *, #1241, .T. ) ;
#7431 = FACE_OUTER_BOUND ( 'NONE', #2655, .T. ) ;
#7432 = ORIENTED_EDGE ( 'NONE', *, *, #3717, .T. ) ;
#7433 = DIRECTION ( 'NONE',  ( -0.000000000000000000, 0.000000000000000000, 1.000000000000000000 ) ) ;
#7434 = CONICAL_SURFACE ( 'NONE', #9173, 37.99999999999999289, 0.7853981633974447263 ) ;
#7435 = AXIS2_PLACEMENT_3D ( 'NONE', #2682, #3336, #6343 ) ;
#7436 = DIRECTION ( 'NONE',  ( -0.000000000000000000, 1.000000000000000000, -0.000000000000000000 ) ) ;
#7437 = CARTESIAN_POINT ( 'NONE',  ( 1.094544505994153880E-26, 56.50000000000029843, -25.00000000000000000 ) ) ;
#7438 = CARTESIAN_POINT ( 'NONE',  ( 5.000000000000008882, 30.00000000000000000, 25.51470164434615029 ) ) ;
#7439 = VERTEX_POINT ( 'NONE', #1767 ) ;
#7440 = DIRECTION ( 'NONE',  ( 0.000000000000000000, 0.000000000000000000, 1.000000000000000000 ) ) ;
#7441 = CARTESIAN_POINT ( 'NONE',  ( 9.654558508304749154, 0.6683215596213600840, 41.54876850399442390 ) ) ;
#7442 = CARTESIAN_POINT ( 'NONE',  ( -8.545448575588393325, 51.50000000000032685, -24.55555555555559621 ) ) ;
#7443 = AXIS2_PLACEMENT_3D ( 'NONE', #3490, #3542, #6498 ) ;
#7444 = CARTESIAN_POINT ( 'NONE',  ( 8.677469957431129860E-27, 43.00000000000019895, -26.00000000000015987 ) ) ;
#7445 = DIRECTION ( 'NONE',  ( -0.9860132971832694659, -1.788557213313974350E-28, 0.1666666666666658247 ) ) ;
#7446 = EDGE_CURVE ( 'NONE', #5699, #7580, #7932, .T. ) ;
#7447 = CARTESIAN_POINT ( 'NONE',  ( 5.562309845534932684, 61.83753588906734677, -37.56426808735049150 ) ) ;
#7448 = AXIS2_PLACEMENT_3D ( 'NONE', #2355, #8345, #4702 ) ;
#7449 = CARTESIAN_POINT ( 'NONE',  ( 31.00000000000001066, 27.95223080783002345, -1.991564994335478067 ) ) ;
#7450 = CARTESIAN_POINT ( 'NONE',  ( 2.400000000000000799, 0.000000000000000000, 0.000000000000000000 ) ) ;
#7451 = ORIENTED_EDGE ( 'NONE', *, *, #9262, .F. ) ;
#7452 = DIRECTION ( 'NONE',  ( 0.000000000000000000, 0.000000000000000000, 1.000000000000000000 ) ) ;
#7453 = CARTESIAN_POINT ( 'NONE',  ( 7.745102572868511004, -15.00000000000000178, 36.88861640503655792 ) ) ;
#7454 = AXIS2_PLACEMENT_3D ( 'NONE', #9239, #7099, #6358 ) ;
#7455 = ORIENTED_EDGE ( 'NONE', *, *, #4474, .T. ) ;
#7456 = ADVANCED_FACE ( 'NONE', ( #8589 ), #2547, .T. ) ;
#7457 = EDGE_CURVE ( 'NONE', #5928, #6521, #9016, .T. ) ;
#7458 = EDGE_CURVE ( 'NONE', #909, #9368, #6451, .T. ) ;
#7459 = PLANE ( 'NONE',  #6006 ) ;
#7460 = DIRECTION ( 'NONE',  ( 0.000000000000000000, 1.000000000000000000, 0.000000000000000000 ) ) ;
#7461 = VERTEX_POINT ( 'NONE', #3493 ) ;
#7462 = AXIS2_PLACEMENT_3D ( 'NONE', #1940, #7124, #7069 ) ;
#7463 = VECTOR ( 'NONE', #2757, 1000.000000000000000 ) ;
#7464 = CARTESIAN_POINT ( 'NONE',  ( 9.671751807051032657, 0.7110059823529706335, 37.94088100612616898 ) ) ;
#7465 = SHAPE_DEFINITION_REPRESENTATION ( #1577, #490 ) ;
#7466 = EDGE_LOOP ( 'NONE', ( #5247, #2946, #8314, #7512 ) ) ;
#7467 = LINE ( 'NONE', #2552, #2133 ) ;
#7468 = ORIENTED_EDGE ( 'NONE', *, *, #3765, .F. ) ;
#7469 = CARTESIAN_POINT ( 'NONE',  ( 34.95336322954870667, 59.50565096299369827, 3.917041198934863022 ) ) ;
#7470 = ORIENTED_EDGE ( 'NONE', *, *, #4998, .F. ) ;
#7471 = CARTESIAN_POINT ( 'NONE',  ( 1.300000000000000044, -0.7216878364870318308, 1.250000000000000000 ) ) ;
#7472 = ORIENTED_EDGE ( 'NONE', *, *, #8007, .F. ) ;
#7473 = CARTESIAN_POINT ( 'NONE',  ( -8.114530083417154316, 9.147922986853130212, 42.28388318272966018 ) ) ;
#7474 = CARTESIAN_POINT ( 'NONE',  ( 0.000000000000000000, 59.99999999999999289, 0.000000000000000000 ) ) ;
#7475 = DIRECTION ( 'NONE',  ( 0.000000000000000000, 0.000000000000000000, 1.000000000000000000 ) ) ;
#7476 = ORIENTED_EDGE ( 'NONE', *, *, #8375, .T. ) ;
#7477 = DIRECTION ( 'NONE',  ( 0.000000000000000000, -1.000000000000000000, 0.000000000000000000 ) ) ;
#7478 = EDGE_LOOP ( 'NONE', ( #9491, #4003, #4025, #2061 ) ) ;
#7479 = LINE ( 'NONE', #5942, #1729 ) ;
#7480 = LINE ( 'NONE', #4384, #3795 ) ;
#7481 = DIRECTION ( 'NONE',  ( -1.820952055660014662E-28, -1.000000000000000000, -7.038118388768679669E-30 ) ) ;
#7482 = AXIS2_PLACEMENT_3D ( 'NONE', #6825, #4529, #5410 ) ;
#7483 = CONICAL_SURFACE ( 'NONE', #3532, 1732.050807568856271, 1.047197551196592524 ) ;
#7484 = CARTESIAN_POINT ( 'NONE',  ( 10.65363874401993982, -5.269189486186425242, 37.51926849444799217 ) ) ;
#7485 = ADVANCED_FACE ( 'NONE', ( #769 ), #4478, .T. ) ;
#7486 = CYLINDRICAL_SURFACE ( 'NONE', #2667, 38.00000000000000711 ) ;
#7487 = CIRCLE ( 'NONE', #6527, 27.00000000000000355 ) ;
#7488 = EDGE_LOOP ( 'NONE', ( #1145, #9584, #7770, #1337, #5406 ) ) ;
#7489 = CARTESIAN_POINT ( 'NONE',  ( 9.999999999999857891, 2.629206769140929989, 41.36423575989298485 ) ) ;
#7490 = CARTESIAN_POINT ( 'NONE',  ( 0.8972019489733558117, -14.99999999999999822, 30.49724508152266367 ) ) ;
#7491 = DIRECTION ( 'NONE',  ( 1.735493991486228494E-29, 0.000000000000000000, -1.000000000000000000 ) ) ;
#7492 = EDGE_CURVE ( 'NONE', #2210, #7105, #6501, .T. ) ;
#7493 = PLANE ( 'NONE',  #9533 ) ;
#7494 = AXIS2_PLACEMENT_3D ( 'NONE', #4062, #3359, #4894 ) ;
#7495 = VECTOR ( 'NONE', #6839, 1000.000000000000000 ) ;
#7496 = CARTESIAN_POINT ( 'NONE',  ( 18.58791755254457811, 59.99999999999999289, 23.54759692749571443 ) ) ;
#7497 = DIRECTION ( 'NONE',  ( 1.820952055660014662E-28, 1.000000000000000000, 7.038118388768679669E-30 ) ) ;
#7498 = CIRCLE ( 'NONE', #5302, 1.249999999999999778 ) ;
#7499 = AXIS2_PLACEMENT_3D ( 'NONE', #5062, #5112, #5206 ) ;
#7500 = DIRECTION ( 'NONE',  ( -1.820952055660014662E-28, -1.000000000000000000, -7.038118388768679669E-30 ) ) ;
#7501 = VECTOR ( 'NONE', #8972, 1000.000000000000341 ) ;
#7502 = VECTOR ( 'NONE', #3574, 1000.000000000000000 ) ;
#7503 = ORIENTED_EDGE ( 'NONE', *, *, #5657, .T. ) ;
#7504 = DIRECTION ( 'NONE',  ( 0.7071067811865573427, 0.7071067811865376918, 0.000000000000000000 ) ) ;
#7505 = DIRECTION ( 'NONE',  ( 0.000000000000000000, 1.000000000000000000, 0.000000000000000000 ) ) ;
#7506 = ORIENTED_EDGE ( 'NONE', *, *, #3050, .F. ) ;
#7507 = ADVANCED_FACE ( 'NONE', ( #7200 ), #1962, .F. ) ;
#7508 = EDGE_CURVE ( 'NONE', #1296, #1637, #4988, .T. ) ;
#7509 = CARTESIAN_POINT ( 'NONE',  ( -33.06426808735054124, 60.99999999999999289, -5.562309845534586294 ) ) ;
#7510 = AXIS2_PLACEMENT_3D ( 'NONE', #857, #802, #3813 ) ;
#7511 = DIRECTION ( 'NONE',  ( 0.000000000000000000, 0.000000000000000000, -1.000000000000000000 ) ) ;
#7512 = ORIENTED_EDGE ( 'NONE', *, *, #3597, .F. ) ;
#7513 = CARTESIAN_POINT ( 'NONE',  ( 9.932836106771395279, 1.962987939473650245, 41.40115169427811992 ) ) ;
#7514 = EDGE_CURVE ( 'NONE', #3045, #6709, #3547, .T. ) ;
#7515 = APPLICATION_PROTOCOL_DEFINITION ( 'draft international standard', 'automotive_design', 1998, #2575 ) ;
#7516 = ORIENTED_EDGE ( 'NONE', *, *, #1515, .T. ) ;
#7517 = CARTESIAN_POINT ( 'NONE',  ( 35.86802812777743554, 61.99999999999999289, 9.082100980773358145 ) ) ;
#7518 = EDGE_CURVE ( 'NONE', #8065, #3624, #8000, .T. ) ;
#7519 = VECTOR ( 'NONE', #3543, 1000.000000000000000 ) ;
#7520 = CARTESIAN_POINT ( 'NONE',  ( 8.283039504820623957E-27, 47.00000000000034106, -26.00000000000012790 ) ) ;
#7521 = DIRECTION ( 'NONE',  ( 0.000000000000000000, 0.000000000000000000, -1.000000000000000000 ) ) ;
#7522 = ORIENTED_EDGE ( 'NONE', *, *, #9032, .F. ) ;
#7523 = LINE ( 'NONE', #9150, #7834 ) ;
#7524 = VERTEX_POINT ( 'NONE', #8789 ) ;
#7525 = CARTESIAN_POINT ( 'NONE',  ( 4.653657836759941152E-15, 39.99999999999999289, 37.99999999999999289 ) ) ;
#7526 = CARTESIAN_POINT ( 'NONE',  ( -5.137569555611031014, 60.99999999999999289, -32.59762842694632212 ) ) ;
#7527 = PLANE ( 'NONE',  #8410 ) ;
#7528 = EDGE_CURVE ( 'NONE', #1935, #2408, #2009, .T. ) ;
#7529 = EDGE_CURVE ( 'NONE', #2848, #4270, #8093, .T. ) ;
#7530 = VECTOR ( 'NONE', #7635, 1000.000000000000114 ) ;
#7531 = ORIENTED_EDGE ( 'NONE', *, *, #4563, .T. ) ;
#7532 = CARTESIAN_POINT ( 'NONE',  ( 33.06426808735054124, 59.99576382555915899, 3.062309845534584074 ) ) ;
#7533 = ADVANCED_FACE ( 'NONE', ( #5262 ), #4532, .T. ) ;
#7534 = VERTEX_POINT ( 'NONE', #6729 ) ;
#7535 = UNCERTAINTY_MEASURE_WITH_UNIT (LENGTH_MEASURE( 1.000000000000000082E-05 ), #2749, 'distance_accuracy_value', 'NONE');
#7536 = ORIENTED_EDGE ( 'NONE', *, *, #226, .F. ) ;
#7537 = PLANE ( 'NONE',  #4414 ) ;
#7538 = SHAPE_REPRESENTATION_RELATIONSHIP ( 'NONE' , 'NONE' ,  #5213, #9748 ) ;
#7539 = DIRECTION ( 'NONE',  ( -0.000000000000000000, -1.000000000000000000, -0.000000000000000000 ) ) ;
#7540 = CARTESIAN_POINT ( 'NONE',  ( 31.00000000000000711, -15.00000000000000000, -6.000000000000006217 ) ) ;
#7541 = DIRECTION ( 'NONE',  ( -0.9449569463147374782, 0.000000000000000000, -0.3271946967961527619 ) ) ;
#7542 = VERTEX_POINT ( 'NONE', #5817 ) ;
#7543 = LINE ( 'NONE', #186, #9161 ) ;
#7544 = CARTESIAN_POINT ( 'NONE',  ( -5.206952648169303366, 59.04364549838359721, 35.56426808735298550 ) ) ;
#7545 = ORIENTED_EDGE ( 'NONE', *, *, #8959, .F. ) ;
#7546 = CARTESIAN_POINT ( 'NONE',  ( -9.082100980773482490, 61.99999999999999289, 35.86802812777740002 ) ) ;
#7547 = FACE_OUTER_BOUND ( 'NONE', #2310, .T. ) ;
#7548 = CARTESIAN_POINT ( 'NONE',  ( -15.97678174684350871, 61.99999999999999289, 30.37459861216651191 ) ) ;
#7549 = CARTESIAN_POINT ( 'NONE',  ( 1.427024630974435215, -14.99999999999999645, 30.38141360069620234 ) ) ;
#7550 = CARTESIAN_POINT ( 'NONE',  ( -8.545448575588403983, -1.753944400353455691E-27, -24.55555555555566727 ) ) ;
#7551 = FACE_OUTER_BOUND ( 'NONE', #920, .T. ) ;
#7552 = ORIENTED_EDGE ( 'NONE', *, *, #7007, .F. ) ;
#7553 = CARTESIAN_POINT ( 'NONE',  ( -3.512770744807076184, 17.76626513302256072, 38.84267909417927456 ) ) ;
#7554 = EDGE_CURVE ( 'NONE', #8960, #7666, #9006, .T. ) ;
#7555 = CARTESIAN_POINT ( 'NONE',  ( 0.000000000000000000, 59.99999999999999289, -37.00000000000000711 ) ) ;
#7556 = CARTESIAN_POINT ( 'NONE',  ( 0.000000000000000000, 0.000000000000000000, 0.000000000000000000 ) ) ;
#7557 = EDGE_LOOP ( 'NONE', ( #410, #2690, #2816, #1151 ) ) ;
#7558 = FACE_OUTER_BOUND ( 'NONE', #801, .T. ) ;
#7559 = CARTESIAN_POINT ( 'NONE',  ( 2.584928722267243906, -9.213195917623087539, 39.41233310064572493 ) ) ;
#7560 = EDGE_LOOP ( 'NONE', ( #3808, #8951, #3009, #3117, #9305 ) ) ;
#7561 = CARTESIAN_POINT ( 'NONE',  ( -30.00000000000001066, 59.99999999999999289, -3.142333204958820777E-13 ) ) ;
#7562 = DIRECTION ( 'NONE',  ( -1.000000000000000000, 0.000000000000000000, 0.000000000000000000 ) ) ;
#7563 = ORIENTED_EDGE ( 'NONE', *, *, #7774, .F. ) ;
#7564 = CARTESIAN_POINT ( 'NONE',  ( 13.29631672938959497, 3.758523381800037200, 36.66344176870511973 ) ) ;
#7565 = EDGE_CURVE ( 'NONE', #1409, #960, #2054, .T. ) ;
#7566 = ORIENTED_EDGE ( 'NONE', *, *, #2945, .F. ) ;
#7567 = CARTESIAN_POINT ( 'NONE',  ( 6.000000000000001776, -15.00000000000000000, -31.00000000000000711 ) ) ;
#7568 = CARTESIAN_POINT ( 'NONE',  ( -4.665243217607698334, 29.66524321760768501, 25.23917843705063646 ) ) ;
#7569 = EDGE_LOOP ( 'NONE', ( #2359, #3428 ) ) ;
#7570 = CARTESIAN_POINT ( 'NONE',  ( 33.06426808735053413, 59.89212256466219486, 8.062309845534588959 ) ) ;
#7571 = ORIENTED_EDGE ( 'NONE', *, *, #4929, .F. ) ;
#7572 = CARTESIAN_POINT ( 'NONE',  ( -8.654999523778794668, 8.345309360148107203, 42.04488323937489724 ) ) ;
#7573 = AXIS2_PLACEMENT_3D ( 'NONE', #1879, #4903, #4169 ) ;
#7574 = CARTESIAN_POINT ( 'NONE',  ( 5.562309845534588959, 49.99999999999999289, -33.06426808735054124 ) ) ;
#7575 = CARTESIAN_POINT ( 'NONE',  ( -3.517955418139367740, 61.99189485091269347, 37.07865250164484650 ) ) ;
#7576 = VECTOR ( 'NONE', #7839, 1000.000000000000000 ) ;
#7577 = ORIENTED_EDGE ( 'NONE', *, *, #5319, .T. ) ;
#7578 = CARTESIAN_POINT ( 'NONE',  ( -1.061959934010897166, -9.435780383690808293, 39.51211129341553630 ) ) ;
#7579 = ORIENTED_EDGE ( 'NONE', *, *, #1609, .F. ) ;
#7580 = VERTEX_POINT ( 'NONE', #4294 ) ;
#7581 = CARTESIAN_POINT ( 'NONE',  ( -2.212457605706169339, -6.470654839585223250, 38.95887210749778973 ) ) ;
#7582 = EDGE_CURVE ( 'NONE', #4514, #9543, #6183, .T. ) ;
#7583 = EDGE_CURVE ( 'NONE', #7681, #3498, #1610, .T. ) ;
#7584 = AXIS2_PLACEMENT_3D ( 'NONE', #5894, #6675, #722 ) ;
#7585 = EDGE_CURVE ( 'NONE', #1595, #8444, #1702, .T. ) ;
#7586 = CARTESIAN_POINT ( 'NONE',  ( 0.000000000000000000, 0.7216878364870328300, -1.250000000000000000 ) ) ;
#7587 = ORIENTED_EDGE ( 'NONE', *, *, #6251, .F. ) ;
#7588 = LINE ( 'NONE', #1612, #7728 ) ;
#7589 = DIRECTION ( 'NONE',  ( 0.000000000000000000, 0.000000000000000000, 1.000000000000000000 ) ) ;
#7590 = VERTEX_POINT ( 'NONE', #1650 ) ;
#7591 = CARTESIAN_POINT ( 'NONE',  ( -5.902069945235074222, 61.82045560759793545, 37.56426808735054124 ) ) ;
#7592 = CARTESIAN_POINT ( 'NONE',  ( 8.476794693501936706, -2.020196700696827108, 42.12368207434300160 ) ) ;
#7593 = CARTESIAN_POINT ( 'NONE',  ( 0.000000000000000000, 58.99999999999999289, 0.000000000000000000 ) ) ;
#7594 = CARTESIAN_POINT ( 'NONE',  ( 1.300000000000000044, 0.000000000000000000, 0.000000000000000000 ) ) ;
#7595 = CARTESIAN_POINT ( 'NONE',  ( 0.000000000000000000, 3.294852476641296768, 295.0000000000000000 ) ) ;
#7596 = PRESENTATION_STYLE_ASSIGNMENT (( #1569 ) ) ;
#7597 = CARTESIAN_POINT ( 'NONE',  ( 2.021687836487040535, 2.168404344971008868E-16, 0.000000000000000000 ) ) ;
#7598 = EDGE_LOOP ( 'NONE', ( #4683, #4147 ) ) ;
#7599 = DIRECTION ( 'NONE',  ( -0.000000000000000000, -1.000000000000000000, -0.000000000000000000 ) ) ;
#7600 = PRODUCT_DEFINITION_FORMATION_WITH_SPECIFIED_SOURCE ( 'ANY', '', #8602, .NOT_KNOWN. ) ;
#7601 = ORIENTED_EDGE ( 'NONE', *, *, #3284, .F. ) ;
#7602 = DIRECTION ( 'NONE',  ( 0.7849198975831893632, -0.000000000000000000, -0.6195972517514871658 ) ) ;
#7603 = ORIENTED_EDGE ( 'NONE', *, *, #4862, .F. ) ;
#7604 = LINE ( 'NONE', #4648, #533 ) ;
#7605 = CARTESIAN_POINT ( 'NONE',  ( 2.461798344461688437, -15.00000000000000000, 30.03527913442230712 ) ) ;
#7606 = VERTEX_POINT ( 'NONE', #6971 ) ;
#7607 = AXIS2_PLACEMENT_3D ( 'NONE', #3362, #312, #1924 ) ;
#7608 = FACE_OUTER_BOUND ( 'NONE', #3187, .T. ) ;
#7609 = CARTESIAN_POINT ( 'NONE',  ( 9.762153702110021092E-27, 46.00000000000018474, -37.00000000000000711 ) ) ;
#7610 = VERTEX_POINT ( 'NONE', #2476 ) ;
#7611 = CARTESIAN_POINT ( 'NONE',  ( 9.331651614526968785, -0.3404697570833234432, 38.02245871504709385 ) ) ;
#7612 = CONTEXT_DEPENDENT_SHAPE_REPRESENTATION ( #7318, #9070 ) ;
#7613 = ORIENTED_EDGE ( 'NONE', *, *, #7146, .F. ) ;
#7614 = FACE_OUTER_BOUND ( 'NONE', #8903, .T. ) ;
#7615 = CARTESIAN_POINT ( 'NONE',  ( -8.216777476527294510, 46.00000000000018474, -23.61111111111111427 ) ) ;
#7616 = VERTEX_POINT ( 'NONE', #6922 ) ;
#7617 = CARTESIAN_POINT ( 'NONE',  ( 0.000000000000000000, 3.294852476641296768, 184.6745183374407020 ) ) ;
#7618 = ORIENTED_EDGE ( 'NONE', *, *, #1978, .T. ) ;
#7619 = CARTESIAN_POINT ( 'NONE',  ( 6.000000000000001776, 30.00000000000000000, -28.37252191822216218 ) ) ;
#7620 = CARTESIAN_POINT ( 'NONE',  ( -25.51470164434615029, 30.00000000000000000, -4.999999999999997335 ) ) ;
#7621 = VECTOR ( 'NONE', #8211, 1000.000000000000114 ) ;
#7622 = LINE ( 'NONE', #2416, #2238 ) ;
#7623 = AXIS2_PLACEMENT_3D ( 'NONE', #8393, #692, #896 ) ;
#7624 = EDGE_LOOP ( 'NONE', ( #6445, #1320, #4815, #6574 ) ) ;
#7625 = DIRECTION ( 'NONE',  ( 0.3271946967961538166, 0.000000000000000000, -0.9449569463147371451 ) ) ;
#7626 = ORIENTED_EDGE ( 'NONE', *, *, #8838, .F. ) ;
#7627 = EDGE_LOOP ( 'NONE', ( #5800, #5233, #141, #4011 ) ) ;
#7628 = CARTESIAN_POINT ( 'NONE',  ( -0.02945139436736224012, -11.70511861050984947, 43.99999014335539016 ) ) ;
#7629 = FACE_OUTER_BOUND ( 'NONE', #2930, .T. ) ;
#7630 = ORIENTED_EDGE ( 'NONE', *, *, #889, .F. ) ;
#7631 = DIRECTION ( 'NONE',  ( 0.000000000000000000, 0.000000000000000000, 1.000000000000000000 ) ) ;
#7632 = CARTESIAN_POINT ( 'NONE',  ( 3.070933240276034759, 59.99999999999999289, -32.85680095556730862 ) ) ;
#7633 = ADVANCED_FACE ( 'NONE', ( #872 ), #2225, .T. ) ;
#7634 = EDGE_LOOP ( 'NONE', ( #3079, #9702, #9472, #8071 ) ) ;
#7635 = DIRECTION ( 'NONE',  ( -1.301620493614667237E-28, -0.7021094974994117610, 0.7120689949163097054 ) ) ;
#7636 = EDGE_CURVE ( 'NONE', #3019, #6432, #9030, .T. ) ;
#7637 = CYLINDRICAL_SURFACE ( 'NONE', #3406, 34.50000000000000000 ) ;
#7638 = DIRECTION ( 'NONE',  ( 0.000000000000000000, 0.000000000000000000, 1.000000000000000000 ) ) ;
#7639 = SURFACE_SIDE_STYLE ('',( #972 ) ) ;
#7640 = AXIS2_PLACEMENT_3D ( 'NONE', #6784, #1458, #731 ) ;
#7641 = PLANE ( 'NONE',  #492 ) ;
#7642 = ORIENTED_EDGE ( 'NONE', *, *, #4716, .F. ) ;
#7643 = CARTESIAN_POINT ( 'NONE',  ( -31.00000000000000711, -15.00000000000000000, 6.000000000000009770 ) ) ;
#7644 = VECTOR ( 'NONE', #5028, 1000.000000000000114 ) ;
#7645 = VECTOR ( 'NONE', #8237, 999.9999999999998863 ) ;
#7646 = ADVANCED_FACE ( 'NONE', ( #7629 ), #5417, .F. ) ;
#7647 = CARTESIAN_POINT ( 'NONE',  ( 0.000000000000000000, 52.29648987751954792, 0.000000000000000000 ) ) ;
#7648 = PRODUCT_DEFINITION_SHAPE ( 'NONE', 'NONE',  #9762 ) ;
#7649 = EDGE_CURVE ( 'NONE', #1665, #6026, #5088, .T. ) ;
#7650 = EDGE_LOOP ( 'NONE', ( #6315, #6426, #9674, #912 ) ) ;
#7651 = CARTESIAN_POINT ( 'NONE',  ( 26.32489316217636954, -10.00000000000000533, -6.000000000000006217 ) ) ;
#7652 = CARTESIAN_POINT ( 'NONE',  ( 37.08058572124223673, 61.87769929713620343, 7.610216775991024640 ) ) ;
#7653 = VERTEX_POINT ( 'NONE', #2334 ) ;
#7654 = AXIS2_PLACEMENT_3D ( 'NONE', #3568, #2162, #9544 ) ;
#7655 = VECTOR ( 'NONE', #2445, 1000.000000000000000 ) ;
#7656 = FACE_OUTER_BOUND ( 'NONE', #6820, .T. ) ;
#7657 = LINE ( 'NONE', #901, #1348 ) ;
#7658 = ORIENTED_EDGE ( 'NONE', *, *, #8073, .T. ) ;
#7659 = CIRCLE ( 'NONE', #2594, 37.99999999999999289 ) ;
#7660 = CIRCLE ( 'NONE', #9408, 26.00000000000003197 ) ;
#7661 = CARTESIAN_POINT ( 'NONE',  ( -8.545448575588380891, 53.50000000000031264, -24.55555555555556779 ) ) ;
#7662 = CARTESIAN_POINT ( 'NONE',  ( 6.656046503713715090, -9.726635889951044334, 38.43478818343638181 ) ) ;
#7663 = CIRCLE ( 'NONE', #417, 3.799999999999999378 ) ;
#7664 = ITEM_DEFINED_TRANSFORMATION ( 'NONE', 'NONE', #2203,  #6314 ) ;
#7665 = AXIS2_PLACEMENT_3D ( 'NONE', #1211, #4177, #5697 ) ;
#7666 = VERTEX_POINT ( 'NONE', #3123 ) ;
#7667 = LINE ( 'NONE', #6861, #6398 ) ;
#7668 = CARTESIAN_POINT ( 'NONE',  ( 8.934430193578387011E-27, 49.00000000000032685, 3.243266026348105177E-28 ) ) ;
#7669 = ORIENTED_EDGE ( 'NONE', *, *, #3586, .T. ) ;
#7670 = DIRECTION ( 'NONE',  ( 0.000000000000000000, 1.000000000000000000, -0.000000000000000000 ) ) ;
#7671 = ORIENTED_EDGE ( 'NONE', *, *, #7076, .T. ) ;
#7672 = CIRCLE ( 'NONE', #8140, 25.00000000000000000 ) ;
#7673 = AXIS2_PLACEMENT_3D ( 'NONE', #6118, #904, #162 ) ;
#7674 = FACE_OUTER_BOUND ( 'NONE', #8752, .T. ) ;
#7675 = ADVANCED_FACE ( 'NONE', ( #4678 ), #5511, .F. ) ;
#7676 = CARTESIAN_POINT ( 'NONE',  ( -9.656652801210938719, 0.6761216413562457506, 41.54767058179530181 ) ) ;
#7677 = VECTOR ( 'NONE', #8585, 1000.000000000000000 ) ;
#7678 = ORIENTED_EDGE ( 'NONE', *, *, #7049, .F. ) ;
#7679 = ORIENTED_EDGE ( 'NONE', *, *, #3712, .F. ) ;
#7680 = CYLINDRICAL_SURFACE ( 'NONE', #1350, 4.500000000000003553 ) ;
#7681 = VERTEX_POINT ( 'NONE', #3224 ) ;
#7682 = VERTEX_POINT ( 'NONE', #5363 ) ;
#7683 = DIRECTION ( 'NONE',  ( 1.735493991486225972E-29, -6.508102468073347395E-30, -1.000000000000000000 ) ) ;
#7684 = DIRECTION ( 'NONE',  ( -1.000000000000000000, -0.000000000000000000, -0.000000000000000000 ) ) ;
#7685 = ORIENTED_EDGE ( 'NONE', *, *, #6762, .T. ) ;
#7686 = DIRECTION ( 'NONE',  ( 0.3271946967961527619, 0.000000000000000000, -0.9449569463147374782 ) ) ;
#7687 = CARTESIAN_POINT ( 'NONE',  ( 0.000000000000000000, 54.99999999999999289, 0.000000000000000000 ) ) ;
#7688 = ORIENTED_EDGE ( 'NONE', *, *, #93, .T. ) ;
#7689 = EDGE_CURVE ( 'NONE', #3235, #2908, #1558, .T. ) ;
#7690 = CARTESIAN_POINT ( 'NONE',  ( 1.093393990668256298E-26, 60.00000000000029843, 3.177784408238939158E-28 ) ) ;
#7691 = CARTESIAN_POINT ( 'NONE',  ( -33.06426808735054124, 59.99999999999999289, -5.562309845534581854 ) ) ;
#7692 = DIRECTION ( 'NONE',  ( 0.000000000000000000, 0.000000000000000000, 1.000000000000000000 ) ) ;
#7693 = CYLINDRICAL_SURFACE ( 'NONE', #2521, 40.00000000000000711 ) ;
#7694 = DIRECTION ( 'NONE',  ( 0.000000000000000000, -0.5000000000000002220, 0.8660254037844384856 ) ) ;
#7695 = ORIENTED_EDGE ( 'NONE', *, *, #7791, .F. ) ;
#7696 = LINE ( 'NONE', #7789, #3228 ) ;
#7697 = EDGE_CURVE ( 'NONE', #7306, #3340, #8519, .T. ) ;
#7698 = CARTESIAN_POINT ( 'NONE',  ( -9.860132971832692661, 39.99999999999999289, -28.33333333333334281 ) ) ;
#7699 = CARTESIAN_POINT ( 'NONE',  ( 0.000000000000000000, 28.99999999999997158, 0.000000000000000000 ) ) ;
#7700 = ORIENTED_EDGE ( 'NONE', *, *, #7704, .F. ) ;
#7701 = LINE ( 'NONE', #9324, #1773 ) ;
#7702 = CARTESIAN_POINT ( 'NONE',  ( 36.08344047792740383, 62.00000000000266454, 8.910509964045653319 ) ) ;
#7703 = ORIENTED_EDGE ( 'NONE', *, *, #2865, .F. ) ;
#7704 = EDGE_CURVE ( 'NONE', #1193, #3027, #8474, .T. ) ;
#7705 = PLANE ( 'NONE',  #358 ) ;
#7706 = B_SPLINE_CURVE_WITH_KNOTS ( 'NONE', 3,
 ( #3067, #178, #23, #6087, #6766, #8469, #6131, #3728, #9009, #3017, #9163, #6027, #1494, #3168, #8415, #2217, #812, #5254 ),
 .UNSPECIFIED., .F., .F.,
 ( 4, 2, 2, 2, 2, 2, 2, 2, 4 ),
 ( 0.000000000000000000, 0.0006356152723216966244, 0.001271230544643393249, 0.001906845816965089873, 0.002542461089286786498, 0.003178076361608482038, 0.003813691633930177578, 0.004449306906251873119, 0.005084922178573568659 ),
 .UNSPECIFIED. ) ;
#7707 = ADVANCED_FACE ( 'NONE', ( #3076 ), #6239, .T. ) ;
#7708 = ADVANCED_FACE ( 'NONE', ( #234 ), #9264, .F. ) ;
#7709 = CARTESIAN_POINT ( 'NONE',  ( 32.59762842694625817, 60.99999999999999289, -5.137569555611371186 ) ) ;
#7710 = VERTEX_POINT ( 'NONE', #7779 ) ;
#7711 = CARTESIAN_POINT ( 'NONE',  ( 2.263813592557596177, -6.451033302730273533, 43.87142663822828581 ) ) ;
#7712 = CARTESIAN_POINT ( 'NONE',  ( 23.54469556655648077, 54.99999999999999289, 29.82695610816123022 ) ) ;
#7713 = DIRECTION ( 'NONE',  ( 0.000000000000000000, 1.000000000000000000, 0.000000000000000000 ) ) ;
#7714 = CARTESIAN_POINT ( 'NONE',  ( 5.008074634385683233, 27.61318074145109591, 31.00000000000000355 ) ) ;
#7715 = VERTEX_POINT ( 'NONE', #9169 ) ;
#7716 = PLANE ( 'NONE',  #8079 ) ;
#7717 = CARTESIAN_POINT ( 'NONE',  ( 1.084683744678891232E-26, 50.50000000000031974, -37.00000000000000711 ) ) ;
#7718 = ORIENTED_EDGE ( 'NONE', *, *, #5710, .T. ) ;
#7719 = CARTESIAN_POINT ( 'NONE',  ( -33.06426808735053413, 59.89212256466219486, -8.062309845534585406 ) ) ;
#7720 = VERTEX_POINT ( 'NONE', #284 ) ;
#7721 = ORIENTED_EDGE ( 'NONE', *, *, #7528, .F. ) ;
#7722 = AXIS2_PLACEMENT_3D ( 'NONE', #6949, #3354, #6360 ) ;
#7723 = PRODUCT_RELATED_PRODUCT_CATEGORY ( 'part', '', ( #2593 ) ) ;
#7724 = VERTEX_POINT ( 'NONE', #140 ) ;
#7725 = DIRECTION ( 'NONE',  ( 0.9999978484633867959, -0.001963425851322921859, 0.0006693485817986371015 ) ) ;
#7726 = FILL_AREA_STYLE_COLOUR ( '', #4354 ) ;
#7727 = DIRECTION ( 'NONE',  ( 0.000000000000000000, 1.000000000000000000, 0.000000000000000000 ) ) ;
#7728 = VECTOR ( 'NONE', #1653, 1000.000000000000000 ) ;
#7729 = ORIENTED_EDGE ( 'NONE', *, *, #9331, .F. ) ;
#7730 = CARTESIAN_POINT ( 'NONE',  ( -16.29881421347314685, 60.99999999999999289, 2.568784777805571906 ) ) ;
#7731 = DIRECTION ( 'NONE',  ( -0.000000000000000000, 1.000000000000000000, -0.000000000000000000 ) ) ;
#7732 = ORIENTED_EDGE ( 'NONE', *, *, #4456, .T. ) ;
#7733 = CARTESIAN_POINT ( 'NONE',  ( -4.000000000000005329, 28.99999999999997158, 0.000000000000000000 ) ) ;
#7734 = CARTESIAN_POINT ( 'NONE',  ( 6.957283601945607465, 59.12244502749634734, -35.14908888799237729 ) ) ;
#7735 = CARTESIAN_POINT ( 'NONE',  ( 33.06426808735054124, 60.99999999999999289, 5.562309845534586294 ) ) ;
#7736 = DIRECTION ( 'NONE',  ( 0.000000000000000000, -0.000000000000000000, 1.000000000000000000 ) ) ;
#7737 = CARTESIAN_POINT ( 'NONE',  ( -29.00000000000000355, 30.00000000000000000, -3.999999999999996447 ) ) ;
#7738 = VERTEX_POINT ( 'NONE', #8421 ) ;
#7739 = AXIS2_PLACEMENT_3D ( 'NONE', #4188, #1222, #4971 ) ;
#7740 = LINE ( 'NONE', #1572, #7495 ) ;
#7741 = CARTESIAN_POINT ( 'NONE',  ( 20.99999999999999645, 28.99999999999997158, -4.000000000000006217 ) ) ;
#7742 = CARTESIAN_POINT ( 'NONE',  ( 31.16666666666653640, 54.99999999999999289, -10.84614626901635503 ) ) ;
#7743 = EDGE_CURVE ( 'NONE', #6478, #5294, #5418, .T. ) ;
#7744 = ORIENTED_EDGE ( 'NONE', *, *, #8209, .F. ) ;
#7745 = FACE_OUTER_BOUND ( 'NONE', #4526, .T. ) ;
#7746 = CARTESIAN_POINT ( 'NONE',  ( 36.86535760663189620, 61.99999999999999289, 3.153634179030289530 ) ) ;
#7747 = VERTEX_POINT ( 'NONE', #820 ) ;
#7748 = DIRECTION ( 'NONE',  ( 0.000000000000000000, 0.000000000000000000, -1.000000000000000000 ) ) ;
#7749 = CARTESIAN_POINT ( 'NONE',  ( -38.00000000000000711, 54.99999999999999289, -3.980288726281173287E-13 ) ) ;
#7750 = ORIENTED_EDGE ( 'NONE', *, *, #8852, .T. ) ;
#7751 = CARTESIAN_POINT ( 'NONE',  ( 33.06426808735054124, 60.99999999999999289, 3.062309845534584074 ) ) ;
#7752 = VERTEX_POINT ( 'NONE', #919 ) ;
#7753 = DIRECTION ( 'NONE',  ( 0.000000000000000000, 1.000000000000000000, 0.000000000000000000 ) ) ;
#7754 = EDGE_CURVE ( 'NONE', #5294, #6478, #1463, .T. ) ;
#7755 = EDGE_CURVE ( 'NONE', #4074, #8381, #434, .T. ) ;
#7756 = ORIENTED_EDGE ( 'NONE', *, *, #4145, .T. ) ;
#7757 = LINE ( 'NONE', #7001, #3064 ) ;
#7758 = VERTEX_POINT ( 'NONE', #324 ) ;
#7759 = CARTESIAN_POINT ( 'NONE',  ( 1.040310318760209318E-26, 50.00000000000032685, -25.00000000000000000 ) ) ;
#7760 = VECTOR ( 'NONE', #7293, 1000.000000000000000 ) ;
#7761 = EDGE_CURVE ( 'NONE', #2719, #1252, #372, .T. ) ;
#7762 = ORIENTED_EDGE ( 'NONE', *, *, #4204, .T. ) ;
#7763 = LINE ( 'NONE', #2563, #2068 ) ;
#7764 = FACE_OUTER_BOUND ( 'NONE', #6529, .T. ) ;
#7765 = AXIS2_PLACEMENT_3D ( 'NONE', #3929, #6281, #86 ) ;
#7766 = DIRECTION ( 'NONE',  ( 0.000000000000000000, 0.000000000000000000, 1.000000000000000000 ) ) ;
#7767 = VERTEX_POINT ( 'NONE', #1062 ) ;
#7768 = CARTESIAN_POINT ( 'NONE',  ( -35.03233509200964590, 59.17868483491578502, -7.112484670352356986 ) ) ;
#7769 = ADVANCED_FACE ( 'NONE', ( #8716 ), #2522, .F. ) ;
#7770 = ORIENTED_EDGE ( 'NONE', *, *, #5766, .T. ) ;
#7771 = CARTESIAN_POINT ( 'NONE',  ( 34.30759795839968262, 59.50675430643739361, 7.737048950318289542 ) ) ;
#7772 = ORIENTED_EDGE ( 'NONE', *, *, #3870, .T. ) ;
#7773 = ORIENTED_EDGE ( 'NONE', *, *, #4986, .T. ) ;
#7774 = EDGE_CURVE ( 'NONE', #6132, #1358, #682, .T. ) ;
#7775 = CARTESIAN_POINT ( 'NONE',  ( -7.316365616915794234, -3.529765552624353209, 42.61083985122122897 ) ) ;
#7776 = VECTOR ( 'NONE', #8644, 1000.000000000000000 ) ;
#7777 = AXIS2_PLACEMENT_3D ( 'NONE', #6405, #3948, #2453 ) ;
#7778 = FACE_OUTER_BOUND ( 'NONE', #3111, .T. ) ;
#7779 = CARTESIAN_POINT ( 'NONE',  ( -25.90235662024527841, 59.99999999999999289, 20.44670930779905049 ) ) ;
#7780 = AXIS2_PLACEMENT_3D ( 'NONE', #7175, #6476, #3374 ) ;
#7781 = ORIENTED_EDGE ( 'NONE', *, *, #5070, .T. ) ;
#7782 = CARTESIAN_POINT ( 'NONE',  ( 1.084683744678891232E-26, 53.00000000000031974, -25.00000000000000000 ) ) ;
#7783 = ORIENTED_EDGE ( 'NONE', *, *, #7182, .F. ) ;
#7784 = CARTESIAN_POINT ( 'NONE',  ( -8.216777476527294510, 59.00000000000029843, -23.61111111111111427 ) ) ;
#7785 = DIRECTION ( 'NONE',  ( 0.000000000000000000, 0.000000000000000000, 1.000000000000000000 ) ) ;
#7786 = CARTESIAN_POINT ( 'NONE',  ( -8.545448575588393325, 45.50000000000019185, -24.55555555555569569 ) ) ;
#7787 = DIRECTION ( 'NONE',  ( 0.000000000000000000, 1.000000000000000000, 0.000000000000000000 ) ) ;
#7788 = CARTESIAN_POINT ( 'NONE',  ( -5.562309845534701758, 60.99999999999999289, 33.06426808735052703 ) ) ;
#7789 = CARTESIAN_POINT ( 'NONE',  ( 1.148778693228098442E-26, 57.50000000000029843, -37.00000000000000711 ) ) ;
#7790 = EDGE_CURVE ( 'NONE', #478, #6987, #9499, .T. ) ;
#7791 = EDGE_CURVE ( 'NONE', #5322, #8683, #6346, .T. ) ;
#7792 = CIRCLE ( 'NONE', #1955, 4.500000000000005329 ) ;
#7793 = CARTESIAN_POINT ( 'NONE',  ( -8.237197373723139648, -15.00000000000000000, 27.80554943579302929 ) ) ;
#7794 = VERTEX_POINT ( 'NONE', #5744 ) ;
#7795 = CYLINDRICAL_SURFACE ( 'NONE', #3993, 2.500000000000002220 ) ;
#7796 = CARTESIAN_POINT ( 'NONE',  ( 0.000000000000000000, 59.99999999999999289, 0.000000000000000000 ) ) ;
#7797 = ORIENTED_EDGE ( 'NONE', *, *, #9698, .F. ) ;
#7798 = CARTESIAN_POINT ( 'NONE',  ( -18.58791755254457456, 59.99999999999999289, -23.54759692749571443 ) ) ;
#7799 = CARTESIAN_POINT ( 'NONE',  ( 16.70299909897254409, 60.99999999999999289, -30.18708036726510002 ) ) ;
#7800 = VECTOR ( 'NONE', #9082, 1000.000000000000000 ) ;
#7801 = AXIS2_PLACEMENT_3D ( 'NONE', #7699, #6254, #894 ) ;
#7802 = CARTESIAN_POINT ( 'NONE',  ( -31.18357922838635687, 59.99999999999999289, -10.79742499427301539 ) ) ;
#7803 = CARTESIAN_POINT ( 'NONE',  ( 5.562309845534933572, 60.99999999999999289, -37.56426808735049150 ) ) ;
#7804 = FACE_OUTER_BOUND ( 'NONE', #688, .T. ) ;
#7805 = VECTOR ( 'NONE', #1871, 1000.000000000000000 ) ;
#7806 = VECTOR ( 'NONE', #2397, 1000.000000000000000 ) ;
#7807 = ORIENTED_EDGE ( 'NONE', *, *, #6598, .T. ) ;
#7808 = CARTESIAN_POINT ( 'NONE',  ( -31.00000000000000711, -10.00000000000000533, -5.999999999999996447 ) ) ;
#7809 = FACE_OUTER_BOUND ( 'NONE', #7221, .T. ) ;
#7810 = ADVANCED_FACE ( 'NONE', ( #2573 ), #5604, .T. ) ;
#7811 = VERTEX_POINT ( 'NONE', #8568 ) ;
#7812 = CARTESIAN_POINT ( 'NONE',  ( -9.815840903884557989, 59.99999999999999289, 28.34870838944214455 ) ) ;
#7813 = AXIS2_PLACEMENT_3D ( 'NONE', #8950, #4408, #7264 ) ;
#7814 = DIRECTION ( 'NONE',  ( 0.9860132971832693549, 1.788449361237088441E-28, -0.1666666666666662133 ) ) ;
#7815 = AXIS2_PLACEMENT_3D ( 'NONE', #777, #9663, #628 ) ;
#7816 = EDGE_CURVE ( 'NONE', #3235, #2792, #1937, .T. ) ;
#7817 = MECHANICAL_DESIGN_GEOMETRIC_PRESENTATION_REPRESENTATION (  '', ( #6071 ), #6235 ) ;
#7818 = EDGE_CURVE ( 'NONE', #5073, #9521, #9121, .T. ) ;
#7819 = CARTESIAN_POINT ( 'NONE',  ( 31.00000000000000711, -15.00000000000000000, -6.000000000000006217 ) ) ;
#7820 = EDGE_LOOP ( 'NONE', ( #2514, #2335, #7587, #481 ) ) ;
#7821 = CARTESIAN_POINT ( 'NONE',  ( -35.54742948121823787, 59.05243086228237104, -5.228649803729171985 ) ) ;
#7822 = ADVANCED_FACE ( 'NONE', ( #8625 ), #1795, .T. ) ;
#7823 = VECTOR ( 'NONE', #3101, 1000.000000000000000 ) ;
#7824 = VERTEX_POINT ( 'NONE', #4178 ) ;
#7825 = CARTESIAN_POINT ( 'NONE',  ( 1.094544505994153880E-26, 60.00000000000029843, -26.01418510567422970 ) ) ;
#7826 = AXIS2_PLACEMENT_3D ( 'NONE', #353, #2461, #5579 ) ;
#7827 = ORIENTED_EDGE ( 'NONE', *, *, #4565, .T. ) ;
#7828 = CIRCLE ( 'NONE', #1041, 39.00000000000002132 ) ;
#7829 = CARTESIAN_POINT ( 'NONE',  ( -13.21233427609164934, 1.350469624994050211, 36.69423386285060928 ) ) ;
#7830 = DIRECTION ( 'NONE',  ( 0.000000000000000000, 0.000000000000000000, 1.000000000000000000 ) ) ;
#7831 = EDGE_CURVE ( 'NONE', #6892, #4799, #3325, .T. ) ;
#7832 = DIRECTION ( 'NONE',  ( -1.000000000000000000, 0.000000000000000000, 0.000000000000000000 ) ) ;
#7833 = ADVANCED_FACE ( 'NONE', ( #6335 ), #4078, .T. ) ;
#7834 = VECTOR ( 'NONE', #3110, 999.9999999999998863 ) ;
#7835 = EDGE_CURVE ( 'NONE', #7876, #1008, #7927, .T. ) ;
#7836 = APPLICATION_CONTEXT ( 'automotive_design' ) ;
#7837 = EDGE_CURVE ( 'NONE', #2117, #3682, #9356, .T. ) ;
#7838 = VERTEX_POINT ( 'NONE', #7227 ) ;
#7839 = DIRECTION ( 'NONE',  ( -0.2340364991664707905, 0.7021094974994116500, -0.6725096063098476851 ) ) ;
#7840 = CARTESIAN_POINT ( 'NONE',  ( -3.147661243663441688, 59.92470504718686897, 33.73534932023822108 ) ) ;
#7841 = ORIENTED_EDGE ( 'NONE', *, *, #3154, .F. ) ;
#7842 = FACE_OUTER_BOUND ( 'NONE', #8223, .T. ) ;
#7843 = CYLINDRICAL_SURFACE ( 'NONE', #2927, 38.00000000000000711 ) ;
#7844 = VECTOR ( 'NONE', #4708, 1000.000000000000000 ) ;
#7845 = DIRECTION ( 'NONE',  ( 0.000000000000000000, -1.000000000000000000, 0.000000000000000000 ) ) ;
#7846 = DIRECTION ( 'NONE',  ( 0.000000000000000000, 1.000000000000000000, 0.000000000000000000 ) ) ;
#7847 = DIRECTION ( 'NONE',  ( -0.000000000000000000, -1.000000000000000000, -0.000000000000000000 ) ) ;
#7848 = CARTESIAN_POINT ( 'NONE',  ( 8.874685183736382811E-27, 44.50000000000019185, -26.00000000000014566 ) ) ;
#7849 = B_SPLINE_CURVE_WITH_KNOTS ( 'NONE', 3,
 ( #3545, #4150, #9577, #2795, #9376, #5816, #2600, #8831, #4843, #4101, #1865, #7145, #1914, #4937, #7949, #7998, #7199, #1179, #4201, #735, #9722, #2944, #5905, #7553, #9029, #6738, #6687, #2889, #5224, #2098 ),
 .UNSPECIFIED., .F., .F.,
 ( 4, 2, 2, 2, 2, 2, 2, 2, 2, 2, 2, 2, 2, 2, 4 ),
 ( 0.01382556044152182841, 0.01776191452666206830, 0.01973009156923219085, 0.02169826861180230992, 0.02366644565437243247, 0.02563462269694255502, 0.02760279973951267757, 0.02957097678208280012, 0.03350733086722303827, 0.03744368495236328337, 0.03941186199493340592, 0.04138003903750352847, 0.04236412755878859321, 0.04334821608007365101, 0.04531639312264377356 ),
 .UNSPECIFIED. ) ;
#7850 = CARTESIAN_POINT ( 'NONE',  ( 2.200000000000000178, 0.000000000000000000, 0.000000000000000000 ) ) ;
#7851 = EDGE_LOOP ( 'NONE', ( #2400, #6299, #1646, #32 ) ) ;
#7852 = PLANE ( 'NONE',  #6153 ) ;
#7853 = DIRECTION ( 'NONE',  ( 0.3286710990610922090, 6.289316826390952918E-29, 0.9444444444444435316 ) ) ;
#7854 = VERTEX_POINT ( 'NONE', #2630 ) ;
#7855 = DIRECTION ( 'NONE',  ( -0.000000000000000000, 1.000000000000000000, -0.000000000000000000 ) ) ;
#7856 = CARTESIAN_POINT ( 'NONE',  ( -2.094888803305880518E-13, 59.99999999999999289, 30.00000000000000711 ) ) ;
#7857 = PRODUCT_RELATED_PRODUCT_CATEGORY ( 'part', '', ( #6053 ) ) ;
#7858 = VERTEX_POINT ( 'NONE', #376 ) ;
#7859 = DIRECTION ( 'NONE',  ( 0.000000000000000000, -0.000000000000000000, 1.000000000000000000 ) ) ;
#7860 = CARTESIAN_POINT ( 'NONE',  ( 5.423418723394456162E-28, -2.066522830327504070E-28, -26.00000000000002132 ) ) ;
#7861 = CARTESIAN_POINT ( 'NONE',  ( 1.138917931912835794E-26, 53.50000000000031264, -37.00000000000000711 ) ) ;
#7862 = CARTESIAN_POINT ( 'NONE',  ( 2.735220335096864019, -6.341052613831273277, 38.93530391522555334 ) ) ;
#7863 = ITEM_DEFINED_TRANSFORMATION ( 'NONE', 'NONE', #8860,  #6314 ) ;
#7864 = CARTESIAN_POINT ( 'NONE',  ( 1.148778693228098442E-26, 57.50000000000029843, -26.00000000000002132 ) ) ;
#7865 = ORIENTED_EDGE ( 'NONE', *, *, #249, .F. ) ;
#7866 = CARTESIAN_POINT ( 'NONE',  ( 32.05305536707737701, 59.99999999999999289, 7.848671329280705322 ) ) ;
#7867 = CARTESIAN_POINT ( 'NONE',  ( 4.007938479032607582, 27.75794689997811204, 31.00000000000000000 ) ) ;
#7868 = ORIENTED_EDGE ( 'NONE', *, *, #3038, .T. ) ;
#7869 = CARTESIAN_POINT ( 'NONE',  ( 0.000000000000000000, 3.294852476641296768, 300.0000000000000000 ) ) ;
#7870 = DIRECTION ( 'NONE',  ( -0.6195972517514869438, 1.387778780781445281E-15, -0.7849198975831893632 ) ) ;
#7871 = ADVANCED_FACE ( 'NONE', ( #5655 ), #1313, .T. ) ;
#7872 = ORIENTED_EDGE ( 'NONE', *, *, #7458, .T. ) ;
#7873 = LINE ( 'NONE', #9452, #103 ) ;
#7874 = ORIENTED_EDGE ( 'NONE', *, *, #9146, .T. ) ;
#7875 = FACE_OUTER_BOUND ( 'NONE', #7228, .T. ) ;
#7876 = VERTEX_POINT ( 'NONE', #5203 ) ;
#7877 = DIRECTION ( 'NONE',  ( -0.000000000000000000, -1.000000000000000000, -0.000000000000000000 ) ) ;
#7878 = VERTEX_POINT ( 'NONE', #2968 ) ;
#7879 = CARTESIAN_POINT ( 'NONE',  ( -9.832659897753353917, 5.164632082215160125, 37.90110321522534065 ) ) ;
#7880 = LINE ( 'NONE', #5743, #264 ) ;
#7881 = CARTESIAN_POINT ( 'NONE',  ( 1.300000000000000044, 3.252606517456513302E-16, 2.499999999999999556 ) ) ;
#7882 = ORIENTED_EDGE ( 'NONE', *, *, #7259, .F. ) ;
#7883 = DIRECTION ( 'NONE',  ( 0.000000000000000000, 0.000000000000000000, 1.000000000000000000 ) ) ;
#7884 = VERTEX_POINT ( 'NONE', #3575 ) ;
#7885 = FACE_OUTER_BOUND ( 'NONE', #3502, .T. ) ;
#7886 = EDGE_CURVE ( 'NONE', #7275, #4788, #2031, .T. ) ;
#7887 = CARTESIAN_POINT ( 'NONE',  ( 0.000000000000000000, 54.99999999999999289, 0.000000000000000000 ) ) ;
#7888 = DIRECTION ( 'NONE',  ( 0.000000000000000000, 1.000000000000000000, 0.000000000000000000 ) ) ;
#7889 = EDGE_CURVE ( 'NONE', #9639, #6883, #4417, .T. ) ;
#7890 = DIRECTION ( 'NONE',  ( -1.000000000000000000, 0.000000000000000000, 0.000000000000000000 ) ) ;
#7891 = EDGE_CURVE ( 'NONE', #7610, #7994, #5937, .T. ) ;
#7892 = CARTESIAN_POINT ( 'NONE',  ( -31.00000000000000711, 27.42469319230600533, 6.000000000000009770 ) ) ;
#7893 = CIRCLE ( 'NONE', #5677, 38.00000000000000711 ) ;
#7894 = AXIS2_PLACEMENT_3D ( 'NONE', #2088, #6586, #6437 ) ;
#7895 = ORIENTED_EDGE ( 'NONE', *, *, #1108, .T. ) ;
#7896 = AXIS2_PLACEMENT_3D ( 'NONE', #4889, #7907, #5072 ) ;
#7897 = PLANE ( 'NONE',  #6837 ) ;
#7898 = ORIENTED_EDGE ( 'NONE', *, *, #4375, .F. ) ;
#7899 = CYLINDRICAL_SURFACE ( 'NONE', #8092, 2.500000000000002220 ) ;
#7900 = CARTESIAN_POINT ( 'NONE',  ( -5.562309845534584518, 59.99999999999999289, 33.06426808735054124 ) ) ;
#7901 = ORIENTED_EDGE ( 'NONE', *, *, #4508, .T. ) ;
#7902 = LINE ( 'NONE', #9435, #1480 ) ;
#7903 = CARTESIAN_POINT ( 'NONE',  ( -1.084202172485504040E-15, 30.00000000000000000, -5.000000000000003553 ) ) ;
#7904 = CIRCLE ( 'NONE', #1899, 34.50000000000000000 ) ;
#7905 = CIRCLE ( 'NONE', #7739, 25.00000000000000000 ) ;
#7906 = CARTESIAN_POINT ( 'NONE',  ( 0.000000000000000000, 39.99999999999999289, 0.000000000000000000 ) ) ;
#7907 = DIRECTION ( 'NONE',  ( 0.000000000000000000, 0.8660254037844385966, -0.5000000000000001110 ) ) ;
#7908 = LINE ( 'NONE', #1087, #1825 ) ;
#7909 = ORIENTED_EDGE ( 'NONE', *, *, #7205, .F. ) ;
#7910 = DIRECTION ( 'NONE',  ( -1.000000000000000000, -0.000000000000000000, -3.491481338843134933E-15 ) ) ;
#7911 = CARTESIAN_POINT ( 'NONE',  ( 33.06426808735054124, 59.99999999999999289, 5.562309845534586294 ) ) ;
#7912 = ORIENTED_EDGE ( 'NONE', *, *, #5522, .T. ) ;
#7913 = DIRECTION ( 'NONE',  ( -0.3286710990610922090, -6.289316826390952918E-29, -0.9444444444444435316 ) ) ;
#7914 = CARTESIAN_POINT ( 'NONE',  ( 24.67792535850613334, 0.000000000000000000, -4.000000000000006217 ) ) ;
#7915 = EDGE_CURVE ( 'NONE', #3824, #1005, #5251, .T. ) ;
#7916 = DIRECTION ( 'NONE',  ( -0.000000000000000000, -1.000000000000000000, -0.000000000000000000 ) ) ;
#7917 = SHAPE_REPRESENTATION_RELATIONSHIP ( 'NONE' , 'NONE' ,  #490, #4453 ) ;
#7918 = AXIS2_PLACEMENT_3D ( 'NONE', #7735, #4781, #6287 ) ;
#7919 = EDGE_LOOP ( 'NONE', ( #8238, #4559, #5981, #4647, #6265 ) ) ;
#7920 = DIRECTION ( 'NONE',  ( 0.000000000000000000, 0.000000000000000000, -1.000000000000000000 ) ) ;
#7921 = ORIENTED_EDGE ( 'NONE', *, *, #7086, .T. ) ;
#7922 = LINE ( 'NONE', #1207, #3879 ) ;
#7923 = ORIENTED_EDGE ( 'NONE', *, *, #4031, .T. ) ;
#7924 = CARTESIAN_POINT ( 'NONE',  ( -9.473662127245630060, 0.07647080102255582323, 41.64234459406086586 ) ) ;
#7925 = DIRECTION ( 'NONE',  ( 0.000000000000000000, 1.000000000000000000, 0.000000000000000000 ) ) ;
#7926 = AXIS2_PLACEMENT_3D ( 'NONE', #1973, #2156, #1243 ) ;
#7927 = LINE ( 'NONE', #4961, #4785 ) ;
#7928 = VERTEX_POINT ( 'NONE', #6669 ) ;
#7929 = PLANE ( 'NONE',  #1892 ) ;
#7930 = ORIENTED_EDGE ( 'NONE', *, *, #3414, .T. ) ;
#7931 = DIRECTION ( 'NONE',  ( -0.000000000000000000, -1.000000000000000000, -0.000000000000000000 ) ) ;
#7932 = CIRCLE ( 'NONE', #8241, 38.00000000000000711 ) ;
#7933 = DIRECTION ( 'NONE',  ( 0.000000000000000000, -1.224646799147353207E-16, 1.000000000000000000 ) ) ;
#7934 = CARTESIAN_POINT ( 'NONE',  ( 13.30448870009049323, 3.640525045295374795, 36.66049983383106792 ) ) ;
#7935 = DIRECTION ( 'NONE',  ( 0.000000000000000000, 0.000000000000000000, 1.000000000000000000 ) ) ;
#7936 = LINE ( 'NONE', #5021, #6999 ) ;
#7937 = VECTOR ( 'NONE', #8167, 1000.000000000000000 ) ;
#7938 = AXIS2_PLACEMENT_3D ( 'NONE', #1177, #2096, #6446 ) ;
#7939 = EDGE_CURVE ( 'NONE', #5005, #1358, #664, .T. ) ;
#7940 = EDGE_CURVE ( 'NONE', #185, #3249, #1304, .T. ) ;
#7941 = CARTESIAN_POINT ( 'NONE',  ( 1.300000000000000044, -0.7216878364870318308, 1.250000000000000000 ) ) ;
#7942 = ORIENTED_EDGE ( 'NONE', *, *, #9014, .F. ) ;
#7943 = EDGE_CURVE ( 'NONE', #4065, #3142, #1398, .T. ) ;
#7944 = CARTESIAN_POINT ( 'NONE',  ( -8.216777476527294510, 40.00000000000014921, -23.61111111111111427 ) ) ;
#7945 = CARTESIAN_POINT ( 'NONE',  ( 8.649757686324669237, 8.323462134889155095, 42.04423075653439668 ) ) ;
#7946 = ORIENTED_EDGE ( 'NONE', *, *, #6762, .F. ) ;
#7947 = CARTESIAN_POINT ( 'NONE',  ( 0.000000000000000000, 3.294852476641296768, 300.0000000000000000 ) ) ;
#7948 = DIRECTION ( 'NONE',  ( 0.000000000000000000, 0.000000000000000000, -1.000000000000000000 ) ) ;
#7949 = CARTESIAN_POINT ( 'NONE',  ( -12.18343812368627255, 9.336105043037195017, 37.04911908969401679 ) ) ;
#7950 = CARTESIAN_POINT ( 'NONE',  ( 5.468730748236366068, -8.297078842874196170, 38.99054534826768048 ) ) ;
#7951 = EDGE_CURVE ( 'NONE', #6352, #5598, #2551, .T. ) ;
#7952 = ADVANCED_FACE ( 'NONE', ( #7378 ), #8728, .F. ) ;
#7953 = CARTESIAN_POINT ( 'NONE',  ( -4.000000000000005329, 28.99999999999997158, -24.67792535850613334 ) ) ;
#7954 = AXIS2_PLACEMENT_3D ( 'NONE', #3333, #3984, #2481 ) ;
#7955 = ORIENTED_EDGE ( 'NONE', *, *, #1950, .F. ) ;
#7956 = LINE ( 'NONE', #4007, #5601 ) ;
#7957 = CARTESIAN_POINT ( 'NONE',  ( -3.817146860096892524, -15.00000000000000000, 29.48174236496974032 ) ) ;
#7958 = ORIENTED_EDGE ( 'NONE', *, *, #4619, .T. ) ;
#7959 =( REPRESENTATION_RELATIONSHIP ('NONE','NONE', #5841, #1483 ) REPRESENTATION_RELATIONSHIP_WITH_TRANSFORMATION ( #9195 )SHAPE_REPRESENTATION_RELATIONSHIP( ) );
#7960 = CARTESIAN_POINT ( 'NONE',  ( -25.90235662024524288, 54.99999999999999289, 20.44670930779909668 ) ) ;
#7961 = DIRECTION ( 'NONE',  ( -0.000000000000000000, 1.000000000000000000, -0.000000000000000000 ) ) ;
#7962 = CARTESIAN_POINT ( 'NONE',  ( 6.823105196324329214, 10.64845247602661082, 38.51605970865411877 ) ) ;
#7963 = CARTESIAN_POINT ( 'NONE',  ( 0.000000000000000000, 0.000000000000000000, 0.000000000000000000 ) ) ;
#7964 = VECTOR ( 'NONE', #1326, 1000.000000000000000 ) ;
#7965 = EDGE_LOOP ( 'NONE', ( #1028, #5241, #8663, #6282, #7064 ) ) ;
#7966 = CARTESIAN_POINT ( 'NONE',  ( -35.86802812777743554, 61.99999999999999289, -9.082100980773358145 ) ) ;
#7967 = ORIENTED_EDGE ( 'NONE', *, *, #2832, .F. ) ;
#7968 = DIRECTION ( 'NONE',  ( -1.820952055660014662E-28, -1.000000000000000000, -7.038118388768679669E-30 ) ) ;
#7969 = ORIENTED_EDGE ( 'NONE', *, *, #3765, .T. ) ;
#7970 = EDGE_LOOP ( 'NONE', ( #4712, #9149, #7417, #6091 ) ) ;
#7971 = CARTESIAN_POINT ( 'NONE',  ( -9.581830020199642917, 0.3921576626816477562, 37.96287317033787900 ) ) ;
#7972 = EDGE_CURVE ( 'NONE', #7406, #5294, #7137, .T. ) ;
#7973 = CIRCLE ( 'NONE', #7494, 30.00000000000000711 ) ;
#7974 = FACE_OUTER_BOUND ( 'NONE', #1884, .T. ) ;
#7975 = AXIS2_PLACEMENT_3D ( 'NONE', #1999, #385, #4141 ) ;
#7976 = CARTESIAN_POINT ( 'NONE',  ( -5.999999999999998224, 29.14236109046821710, 29.24912810952613640 ) ) ;
#7977 = AXIS2_PLACEMENT_3D ( 'NONE', #1925, #5000, #2658 ) ;
#7978 = VECTOR ( 'NONE', #4171, 1000.000000000000000 ) ;
#7979 = ORIENTED_EDGE ( 'NONE', *, *, #8910, .F. ) ;
#7980 = CARTESIAN_POINT ( 'NONE',  ( 0.000000000000000000, 61.99999999999999289, 0.000000000000000000 ) ) ;
#7981 = AXIS2_PLACEMENT_3D ( 'NONE', #8067, #9745, #4374 ) ;
#7982 = ORIENTED_EDGE ( 'NONE', *, *, #8209, .T. ) ;
#7983 = CARTESIAN_POINT ( 'NONE',  ( 0.000000000000000000, -15.00000000000000000, -29.00000000000001776 ) ) ;
#7984 = DIRECTION ( 'NONE',  ( 1.820952055660014662E-28, 1.000000000000000000, -6.508102468073347395E-30 ) ) ;
#7985 = CARTESIAN_POINT ( 'NONE',  ( 6.715732449718500696, 16.24544142831953053, 38.41843156493658995 ) ) ;
#7986 = CARTESIAN_POINT ( 'NONE',  ( 5.562309845534588959, 49.99999999999999289, -33.06426808735054124 ) ) ;
#7987 = CARTESIAN_POINT ( 'NONE',  ( 29.00000000000000355, 30.00000000000000000, -4.000000000000007105 ) ) ;
#7988 = VECTOR ( 'NONE', #2319, 1000.000000000000000 ) ;
#7989 = EDGE_CURVE ( 'NONE', #8408, #6709, #3724, .T. ) ;
#7990 = MECHANICAL_DESIGN_GEOMETRIC_PRESENTATION_REPRESENTATION (  '', ( #3416 ), #8779 ) ;
#7991 = ORIENTED_EDGE ( 'NONE', *, *, #950, .F. ) ;
#7992 = CARTESIAN_POINT ( 'NONE',  ( 0.000000000000000000, 61.99999999999999289, 0.000000000000000000 ) ) ;
#7993 = DIRECTION ( 'NONE',  ( -1.820952055660014662E-28, -1.000000000000000000, 6.508102468073347395E-30 ) ) ;
#7994 = VERTEX_POINT ( 'NONE', #4376 ) ;
#7995 = CARTESIAN_POINT ( 'NONE',  ( 5.421010862427522170E-16, 30.00000000000000000, 5.000000000000004441 ) ) ;
#7996 = DIRECTION ( 'NONE',  ( 0.000000000000000000, 0.000000000000000000, 1.000000000000000000 ) ) ;
#7997 = EDGE_CURVE ( 'NONE', #6613, #5960, #4521, .T. ) ;
#7998 = CARTESIAN_POINT ( 'NONE',  ( -11.40964930878180539, 11.10725308166288983, 37.29763346372921262 ) ) ;
#7999 = ADVANCED_FACE ( 'NONE', ( #3618 ), #2877, .T. ) ;
#8000 = LINE ( 'NONE', #8832, #2545 ) ;
#8001 = VECTOR ( 'NONE', #590, 1000.000000000000000 ) ;
#8002 = DIRECTION ( 'NONE',  ( -0.1666666666666658525, -3.897465909857536228E-29, -0.9860132971832695770 ) ) ;
#8003 = ORIENTED_EDGE ( 'NONE', *, *, #463, .F. ) ;
#8004 = DIRECTION ( 'NONE',  ( 0.3286710990610922090, 6.289316826390952918E-29, 0.9444444444444435316 ) ) ;
#8005 = CARTESIAN_POINT ( 'NONE',  ( -0.3713926049973746979, -15.00000000000000000, 30.56995792405530921 ) ) ;
#8006 = VERTEX_POINT ( 'NONE', #9005 ) ;
#8007 = EDGE_CURVE ( 'NONE', #2949, #2537, #5799, .T. ) ;
#8008 = EDGE_CURVE ( 'NONE', #2208, #3142, #8249, .T. ) ;
#8009 = ADVANCED_FACE ( 'NONE', ( #5160 ), #7527, .F. ) ;
#8010 = DIRECTION ( 'NONE',  ( 0.000000000000000000, 0.000000000000000000, 1.000000000000000000 ) ) ;
#8011 = LINE ( 'NONE', #7213, #3719 ) ;
#8012 = CARTESIAN_POINT ( 'NONE',  ( 8.498720194445880338, 8.574681387762774776, 42.11372032734551141 ) ) ;
#8013 = EDGE_LOOP ( 'NONE', ( #2216, #4681, #4461, #6967 ) ) ;
#8014 = CARTESIAN_POINT ( 'NONE',  ( 0.000000000000000000, 39.99999999999999289, 0.000000000000000000 ) ) ;
#8015 = SPHERICAL_SURFACE ( 'NONE', #1728, 4.324969328314201888 ) ;
#8016 = LINE ( 'NONE', #5835, #3546 ) ;
#8017 = ORIENTED_EDGE ( 'NONE', *, *, #8788, .T. ) ;
#8018 = ORIENTED_EDGE ( 'NONE', *, *, #8538, .F. ) ;
#8019 = CARTESIAN_POINT ( 'NONE',  ( -6.094378065318124982, 11.24985937468323272, 43.04782701210960028 ) ) ;
#8020 = DIRECTION ( 'NONE',  ( -0.000000000000000000, 1.000000000000000000, -0.000000000000000000 ) ) ;
#8021 = CARTESIAN_POINT ( 'NONE',  ( 4.531193156845207581E-15, 58.99999999999999289, 37.00000000000000711 ) ) ;
#8022 = ORIENTED_EDGE ( 'NONE', *, *, #2983, .F. ) ;
#8023 = EDGE_LOOP ( 'NONE', ( #2092, #9002, #489, #4956 ) ) ;
#8024 = CARTESIAN_POINT ( 'NONE',  ( 0.000000000000000000, 30.00000000000000000, 0.000000000000000000 ) ) ;
#8025 = ORIENTED_EDGE ( 'NONE', *, *, #2970, .F. ) ;
#8026 = EDGE_LOOP ( 'NONE', ( #4240, #6973, #3902, #7015 ) ) ;
#8027 = ORIENTED_EDGE ( 'NONE', *, *, #8696, .T. ) ;
#8028 = LINE ( 'NONE', #2086, #5742 ) ;
#8029 = CARTESIAN_POINT ( 'NONE',  ( -33.00000000000000711, 54.99999999999999289, -3.456566525454705682E-13 ) ) ;
#8030 = CARTESIAN_POINT ( 'NONE',  ( 12.05879450961799293, 9.620832044272598083, 37.08913302436281612 ) ) ;
#8031 = DIRECTION ( 'NONE',  ( -0.000000000000000000, -1.000000000000000000, -0.000000000000000000 ) ) ;
#8032 = CARTESIAN_POINT ( 'NONE',  ( 1.555535097482682654E-26, 78.08723716182652197, -25.00000000000000000 ) ) ;
#8033 = EDGE_LOOP ( 'NONE', ( #4309, #6716, #5155, #7979 ) ) ;
#8034 = DIRECTION ( 'NONE',  ( 0.000000000000000000, 0.000000000000000000, 1.000000000000000000 ) ) ;
#8035 = CARTESIAN_POINT ( 'NONE',  ( 5.562309845534932684, 60.99999999999999289, -33.06426808735049150 ) ) ;
#8036 = ORIENTED_EDGE ( 'NONE', *, *, #4928, .T. ) ;
#8037 = CARTESIAN_POINT ( 'NONE',  ( 5.562309845534588959, 49.99999999999999289, -33.06426808735054124 ) ) ;
#8038 = CARTESIAN_POINT ( 'NONE',  ( -4.000000000000005329, 0.000000000000000000, -0.000000000000000000 ) ) ;
#8039 = CIRCLE ( 'NONE', #2822, 3.799999999999999378 ) ;
#8040 = AXIS2_PLACEMENT_3D ( 'NONE', #6248, #1068, #3279 ) ;
#8041 = CARTESIAN_POINT ( 'NONE',  ( 2.204364238465235033E-15, 1.000000000000014655, -17.99999999999999645 ) ) ;
#8042 = DIRECTION ( 'NONE',  ( 1.820952055660014662E-28, 1.000000000000000000, 7.038118388768679669E-30 ) ) ;
#8043 = CIRCLE ( 'NONE', #2043, 33.00000000000000711 ) ;
#8044 = LINE ( 'NONE', #8695, #7324 ) ;
#8045 = ORIENTED_EDGE ( 'NONE', *, *, #9581, .T. ) ;
#8046 = CARTESIAN_POINT ( 'NONE',  ( 0.000000000000000000, 59.99999999999999289, 0.000000000000000000 ) ) ;
#8047 = CARTESIAN_POINT ( 'NONE',  ( -6.507333377502796168, -14.99999999999967848, 36.82578466839068909 ) ) ;
#8048 = EDGE_LOOP ( 'NONE', ( #2984, #6812, #7671, #4407 ) ) ;
#8049 = CIRCLE ( 'NONE', #3315, 34.50000000000000000 ) ;
#8050 = LINE ( 'NONE', #8099, #3015 ) ;
#8051 = B_SPLINE_CURVE_WITH_KNOTS ( 'NONE', 3,
 ( #3892, #970, #6885, #5373, #4780, #8383, #6931, #191, #8482, #1709, #4685, #8426, #7734, #2392, #4587, #4039, #2529, #6195 ),
 .UNSPECIFIED., .F., .F.,
 ( 4, 2, 2, 2, 2, 2, 2, 2, 4 ),
 ( 0.000000000000000000, 0.0006356152723216952150, 0.001271230544643390430, 0.001906845816965085537, 0.002542461089286780860, 0.003178076361608477268, 0.003813691633930173241, 0.004449306906251869649, 0.005084922178573566057 ),
 .UNSPECIFIED. ) ;
#8052 = CARTESIAN_POINT ( 'NONE',  ( 33.06426808735054124, 49.99999999999999289, 8.062309845534588959 ) ) ;
#8053 = CARTESIAN_POINT ( 'NONE',  ( 5.532933570186216343, 16.94308342398178269, 38.60764366510559853 ) ) ;
#8054 = EDGE_CURVE ( 'NONE', #71, #3464, #2779, .T. ) ;
#8055 = EDGE_CURVE ( 'NONE', #8381, #7653, #55, .T. ) ;
#8056 = CARTESIAN_POINT ( 'NONE',  ( 5.562309845534588071, 63.19999999999998153, -33.06426808735054124 ) ) ;
#8057 = CIRCLE ( 'NONE', #3640, 0.2000000000000000944 ) ;
#8058 = ORIENTED_EDGE ( 'NONE', *, *, #8490, .F. ) ;
#8059 = CARTESIAN_POINT ( 'NONE',  ( 1.555535097482682654E-26, 78.08723716182652197, -25.00000000000000000 ) ) ;
#8060 = EDGE_CURVE ( 'NONE', #3135, #2949, #6172, .T. ) ;
#8061 = VERTEX_POINT ( 'NONE', #5353 ) ;
#8062 = DIRECTION ( 'NONE',  ( 0.000000000000000000, 0.000000000000000000, 1.000000000000000000 ) ) ;
#8063 = ORIENTED_EDGE ( 'NONE', *, *, #8838, .T. ) ;
#8064 = LINE ( 'NONE', #4084, #4046 ) ;
#8065 = VERTEX_POINT ( 'NONE', #5308 ) ;
#8066 = DIRECTION ( 'NONE',  ( -1.820952055660014662E-28, -1.000000000000000000, -7.038118388768679669E-30 ) ) ;
#8067 = CARTESIAN_POINT ( 'NONE',  ( 0.000000000000000000, 3.294852476641296768, 294.6136752714472777 ) ) ;
#8068 = AXIS2_PLACEMENT_3D ( 'NONE', #4135, #2528, #4869 ) ;
#8069 = DIRECTION ( 'NONE',  ( -0.3271946967961531505, 0.000000000000000000, 0.9449569463147373671 ) ) ;
#8070 = EDGE_CURVE ( 'NONE', #1345, #1203, #9207, .T. ) ;
#8071 = ORIENTED_EDGE ( 'NONE', *, *, #2956, .F. ) ;
#8072 = CARTESIAN_POINT ( 'NONE',  ( 4.592425496802575156E-15, 59.99999999999999289, 37.00000000000000711 ) ) ;
#8073 = EDGE_CURVE ( 'NONE', #9391, #2731, #7622, .T. ) ;
#8074 = VERTEX_POINT ( 'NONE', #999 ) ;
#8075 = FACE_OUTER_BOUND ( 'NONE', #4463, .T. ) ;
#8076 = DIRECTION ( 'NONE',  ( -1.000000000000000000, -0.000000000000000000, -0.000000000000000000 ) ) ;
#8077 = CARTESIAN_POINT ( 'NONE',  ( 13.22768554207220681, 4.942043779154436933, 36.68828154652676687 ) ) ;
#8078 = DIRECTION ( 'NONE',  ( -0.5000000000000044409, 0.000000000000000000, 0.8660254037844360431 ) ) ;
#8079 = AXIS2_PLACEMENT_3D ( 'NONE', #174, #4663, #6869 ) ;
#8080 = FACE_OUTER_BOUND ( 'NONE', #3600, .T. ) ;
#8081 = AXIS2_PLACEMENT_3D ( 'NONE', #3828, #3980, #3175 ) ;
#8082 = PLANE ( 'NONE',  #7896 ) ;
#8083 = EDGE_LOOP ( 'NONE', ( #9557, #3588, #979, #6880 ) ) ;
#8084 = CARTESIAN_POINT ( 'NONE',  ( -32.21437568466744494, 59.99999999999997868, -7.920020133197000156 ) ) ;
#8085 = CARTESIAN_POINT ( 'NONE',  ( 8.483224498846656303, 8.599388824895884298, 42.12074175542014132 ) ) ;
#8086 = ORIENTED_EDGE ( 'NONE', *, *, #6559, .F. ) ;
#8087 = DIRECTION ( 'NONE',  ( -0.000000000000000000, 1.000000000000000000, -0.000000000000000000 ) ) ;
#8088 = SURFACE_STYLE_USAGE ( .BOTH. , #1278 ) ;
#8089 = FACE_OUTER_BOUND ( 'NONE', #6482, .T. ) ;
#8090 = VECTOR ( 'NONE', #6818, 1000.000000000000000 ) ;
#8091 = ADVANCED_FACE ( 'NONE', ( #7764 ), #1641, .F. ) ;
#8092 = AXIS2_PLACEMENT_3D ( 'NONE', #6353, #9373, #5626 ) ;
#8093 = LINE ( 'NONE', #3025, #5721 ) ;
#8094 = FACE_OUTER_BOUND ( 'NONE', #6376, .T. ) ;
#8095 = ORIENTED_EDGE ( 'NONE', *, *, #6421, .F. ) ;
#8096 = DIRECTION ( 'NONE',  ( -1.735493991486225972E-29, 6.508102468073347395E-30, 1.000000000000000000 ) ) ;
#8097 = CARTESIAN_POINT ( 'NONE',  ( -7.237833666954393230, -7.422220416173621160, 38.57360862901651188 ) ) ;
#8098 = ORIENTED_EDGE ( 'NONE', *, *, #3777, .F. ) ;
#8099 = CARTESIAN_POINT ( 'NONE',  ( 1.097009696322969542E-26, 52.00000000000031974, -25.00000000000000000 ) ) ;
#8100 = DIRECTION ( 'NONE',  ( 1.000000000000000000, 0.000000000000000000, 0.000000000000000000 ) ) ;
#8101 = ORIENTED_EDGE ( 'NONE', *, *, #8845, .T. ) ;
#8102 = CARTESIAN_POINT ( 'NONE',  ( 7.068415056849144840, 10.41224345616790892, 38.47601730954646371 ) ) ;
#8103 = EDGE_CURVE ( 'NONE', #7052, #7811, #5103, .T. ) ;
#8104 = ORIENTED_EDGE ( 'NONE', *, *, #7529, .F. ) ;
#8105 = CARTESIAN_POINT ( 'NONE',  ( -33.40276010569236576, 59.97308474266854716, -3.079737114311556390 ) ) ;
#8106 = EDGE_LOOP ( 'NONE', ( #4134, #9465, #60, #557 ) ) ;
#8107 = CARTESIAN_POINT ( 'NONE',  ( 33.89029069002005912, 59.89318186371823316, 3.196943324609357262 ) ) ;
#8108 = ORIENTED_EDGE ( 'NONE', *, *, #3652, .T. ) ;
#8109 = DIRECTION ( 'NONE',  ( -0.000000000000000000, -1.000000000000000000, -0.000000000000000000 ) ) ;
#8110 = AXIS2_PLACEMENT_3D ( 'NONE', #2243, #1424, #9088 ) ;
#8111 = ORIENTED_EDGE ( 'NONE', *, *, #937, .F. ) ;
#8112 = CARTESIAN_POINT ( 'NONE',  ( -9.980720655645276551, 13.21681672747774883, 37.70234918754850639 ) ) ;
#8113 = LINE ( 'NONE', #8905, #7502 ) ;
#8114 = EDGE_CURVE ( 'NONE', #2298, #1381, #3817, .T. ) ;
#8115 = CARTESIAN_POINT ( 'NONE',  ( -4.999999999999999112, 30.00000000000000000, 29.00000000000000355 ) ) ;
#8116 = AXIS2_PLACEMENT_3D ( 'NONE', #9619, #2842, #8880 ) ;
#8117 = AXIS2_PLACEMENT_3D ( 'NONE', #4398, #7405, #4941 ) ;
#8118 = EDGE_CURVE ( 'NONE', #7838, #2244, #9667, .T. ) ;
#8119 = ORIENTED_EDGE ( 'NONE', *, *, #684, .F. ) ;
#8120 = CARTESIAN_POINT ( 'NONE',  ( 1.555535097482682654E-26, 78.08723716182652197, -25.00000000000000000 ) ) ;
#8121 = DIRECTION ( 'NONE',  ( -0.9444444444444403119, 0.000000000000000000, 0.3286710990611015903 ) ) ;
#8122 = VERTEX_POINT ( 'NONE', #1598 ) ;
#8123 = CARTESIAN_POINT ( 'NONE',  ( 1.040310318760209318E-26, 49.00000000000032685, -37.00000000000000711 ) ) ;
#8124 = CIRCLE ( 'NONE', #5453, 30.00000000000000711 ) ;
#8125 = FACE_OUTER_BOUND ( 'NONE', #2907, .T. ) ;
#8126 = VECTOR ( 'NONE', #6184, 1000.000000000000000 ) ;
#8127 = CARTESIAN_POINT ( 'NONE',  ( 1.300000000000000044, 1.443375672974065216, 1.084202172492522584E-16 ) ) ;
#8128 = ADVANCED_FACE ( 'NONE', ( #175 ), #9157, .F. ) ;
#8129 = LINE ( 'NONE', #2090, #1189 ) ;
#8130 = EDGE_CURVE ( 'NONE', #3288, #9011, #6823, .T. ) ;
#8131 = AXIS2_PLACEMENT_3D ( 'NONE', #4258, #7308, #6608 ) ;
#8132 = AXIS2_PLACEMENT_3D ( 'NONE', #514, #7312, #3510 ) ;
#8133 = AXIS2_PLACEMENT_3D ( 'NONE', #3320, #5550, #4908 ) ;
#8134 = AXIS2_PLACEMENT_3D ( 'NONE', #6382, #7925, #9497 ) ;
#8135 = DIRECTION ( 'NONE',  ( 0.000000000000000000, 1.000000000000000000, 0.000000000000000000 ) ) ;
#8136 = ORIENTED_EDGE ( 'NONE', *, *, #2444, .T. ) ;
#8137 = CARTESIAN_POINT ( 'NONE',  ( 7.557191387046156742E-27, 41.50000000000020606, 2.842672597915560119E-28 ) ) ;
#8138 = FACE_OUTER_BOUND ( 'NONE', #2431, .T. ) ;
#8139 = DIRECTION ( 'NONE',  ( -0.3286710990610922090, -6.289316826390952918E-29, -0.9444444444444435316 ) ) ;
#8140 = AXIS2_PLACEMENT_3D ( 'NONE', #303, #9332, #5577 ) ;
#8141 = LINE ( 'NONE', #5717, #5399 ) ;
#8142 = CARTESIAN_POINT ( 'NONE',  ( 0.000000000000000000, 0.000000000000000000, 0.000000000000000000 ) ) ;
#8143 = FACE_BOUND ( 'NONE', #5336, .T. ) ;
#8144 = VECTOR ( 'NONE', #9741, 1000.000000000000000 ) ;
#8145 = VERTEX_POINT ( 'NONE', #5686 ) ;
#8146 = DIRECTION ( 'NONE',  ( -0.9860132971832694659, -1.788557213313974350E-28, 0.1666666666666658247 ) ) ;
#8147 = PRODUCT_DEFINITION ( 'UNKNOWN', '', #7600, #2771 ) ;
#8148 = ORIENTED_EDGE ( 'NONE', *, *, #5825, .T. ) ;
#8149 = CARTESIAN_POINT ( 'NONE',  ( 0.004085762815451446546, 18.29485247664131009, 39.00000000000001421 ) ) ;
#8150 = CARTESIAN_POINT ( 'NONE',  ( -9.224918227939335580, -6.208428183824680424, 37.97970803284726315 ) ) ;
#8151 = ORIENTED_EDGE ( 'NONE', *, *, #6730, .T. ) ;
#8152 = AXIS2_PLACEMENT_3D ( 'NONE', #734, #8879, #6639 ) ;
#8153 = DIRECTION ( 'NONE',  ( 0.000000000000000000, -0.000000000000000000, 1.000000000000000000 ) ) ;
#8154 = DIRECTION ( 'NONE',  ( -1.000000000000000000, 0.000000000000000000, 0.000000000000000000 ) ) ;
#8155 = ORIENTED_EDGE ( 'NONE', *, *, #9513, .T. ) ;
#8156 = CARTESIAN_POINT ( 'NONE',  ( 7.535708689751818845, 9.876535171860036044, 42.52448306728676641 ) ) ;
#8157 = APPLICATION_PROTOCOL_DEFINITION ( 'draft international standard', 'automotive_design', 1998, #8652 ) ;
#8158 = ORIENTED_EDGE ( 'NONE', *, *, #6173, .F. ) ;
#8159 = DIRECTION ( 'NONE',  ( 1.820952055660014662E-28, 1.000000000000000000, 7.038118388768679669E-30 ) ) ;
#8160 = VERTEX_POINT ( 'NONE', #2509 ) ;
#8161 = CARTESIAN_POINT ( 'NONE',  ( 18.58791755254457811, 39.99999999999999289, 23.54759692749571443 ) ) ;
#8162 = EDGE_LOOP ( 'NONE', ( #9062, #9455, #6284, #2626 ) ) ;
#8163 = DIRECTION ( 'NONE',  ( -1.000000000000000000, 0.000000000000000000, 0.000000000000000000 ) ) ;
#8164 = EDGE_LOOP ( 'NONE', ( #1368, #4325, #15, #763 ) ) ;
#8165 = CARTESIAN_POINT ( 'NONE',  ( -11.92603897288437054, 9.998747279519278663, 37.13350106079722934 ) ) ;
#8166 = DIRECTION ( 'NONE',  ( -1.820952055660014662E-28, -1.000000000000000000, -7.038118388768679669E-30 ) ) ;
#8167 = DIRECTION ( 'NONE',  ( 1.084202172485503325E-16, 0.000000000000000000, 1.000000000000000000 ) ) ;
#8168 = EDGE_LOOP ( 'NONE', ( #6180, #5713, #5671, #5447 ) ) ;
#8169 = CARTESIAN_POINT ( 'NONE',  ( 0.000000000000000000, 0.000000000000000000, 0.000000000000000000 ) ) ;
#8170 = ORIENTED_EDGE ( 'NONE', *, *, #4387, .T. ) ;
#8171 = DIRECTION ( 'NONE',  ( 1.000000000000000000, -0.000000000000000000, 6.982962677686269077E-15 ) ) ;
#8172 = SHAPE_REPRESENTATION_RELATIONSHIP ( 'NONE' , 'NONE' ,  #551, #6085 ) ;
#8173 = DIRECTION ( 'NONE',  ( -0.9860132971832693549, -1.788557213313974126E-28, 0.1666666666666657970 ) ) ;
#8174 = CARTESIAN_POINT ( 'NONE',  ( -32.59762842694629370, 60.99999999999999289, 5.137569555611143812 ) ) ;
#8175 = B_SPLINE_CURVE_WITH_KNOTS ( 'NONE', 3,
 ( #6364, #8600, #1831, #7867, #7714, #7107 ),
 .UNSPECIFIED., .F., .F.,
 ( 4, 2, 4 ),
 ( 0.006018989108141226639, 0.009014550367373157583, 0.01201011162660509113 ),
 .UNSPECIFIED. ) ;
#8176 = CARTESIAN_POINT ( 'NONE',  ( -3.070933240276028542, 59.99999999999999289, 32.85680095556730862 ) ) ;
#8177 = EDGE_CURVE ( 'NONE', #71, #8145, #4791, .T. ) ;
#8178 = B_SPLINE_CURVE_WITH_KNOTS ( 'NONE', 3,
 ( #2369, #5402, #6171, #953 ),
 .UNSPECIFIED., .F., .F.,
 ( 4, 4 ),
 ( 0.000000000000000000, 0.001643226871903046959 ),
 .UNSPECIFIED. ) ;
#8179 = EDGE_CURVE ( 'NONE', #344, #8621, #6029, .T. ) ;
#8180 = ADVANCED_FACE ( 'NONE', ( #9446 ), #7008, .T. ) ;
#8181 = ORIENTED_EDGE ( 'NONE', *, *, #6173, .T. ) ;
#8182 = DIRECTION ( 'NONE',  ( -1.820952055660014662E-28, -1.000000000000000000, -7.038118388768679669E-30 ) ) ;
#8183 = DIRECTION ( 'NONE',  ( -1.000000000000000000, 0.000000000000000000, 0.000000000000000000 ) ) ;
#8184 = PLANE ( 'NONE',  #4672 ) ;
#8185 = EDGE_CURVE ( 'NONE', #5049, #8583, #6370, .T. ) ;
#8186 = DIRECTION ( 'NONE',  ( 0.000000000000000000, 1.000000000000000000, 0.000000000000000000 ) ) ;
#8187 = CARTESIAN_POINT ( 'NONE',  ( 34.07933880998927378, 60.99999999999999289, -5.371095444502794081 ) ) ;
#8188 = DIRECTION ( 'NONE',  ( 0.000000000000000000, 0.000000000000000000, -1.000000000000000000 ) ) ;
#8189 = AXIS2_PLACEMENT_3D ( 'NONE', #7233, #8675, #7280 ) ;
#8190 = FACE_OUTER_BOUND ( 'NONE', #1253, .T. ) ;
#8191 = ORIENTED_EDGE ( 'NONE', *, *, #2862, .F. ) ;
#8192 = FACE_OUTER_BOUND ( 'NONE', #7851, .T. ) ;
#8193 = CARTESIAN_POINT ( 'NONE',  ( 9.147656056445134354, -14.99999999999968558, 37.02405928711753802 ) ) ;
#8194 = EDGE_LOOP ( 'NONE', ( #6673, #9336, #4311, #654, #5245, #6680, #579 ) ) ;
#8195 = CARTESIAN_POINT ( 'NONE',  ( -8.216777476527274970, 78.08723716182652197, -23.61111111111111427 ) ) ;
#8196 = AXIS2_PLACEMENT_3D ( 'NONE', #5321, #8329, #8423 ) ;
#8197 = CARTESIAN_POINT ( 'NONE',  ( 5.562309845534932684, 61.99999999999999289, -33.06426808735049150 ) ) ;
#8198 = ORIENTED_EDGE ( 'NONE', *, *, #5775, .T. ) ;
#8199 = CARTESIAN_POINT ( 'NONE',  ( 7.509679877969126949, -3.381201913332376741, 38.40166088718918047 ) ) ;
#8200 = ORIENTED_EDGE ( 'NONE', *, *, #5358, .T. ) ;
#8201 = CARTESIAN_POINT ( 'NONE',  ( -11.07761026121387538, -4.999999999999996447, 37.39366993089406321 ) ) ;
#8202 = ORIENTED_EDGE ( 'NONE', *, *, #7330, .T. ) ;
#8203 = CARTESIAN_POINT ( 'NONE',  ( 1.045240699417840642E-26, 47.50000000000033396, -37.00000000000000711 ) ) ;
#8204 = VERTEX_POINT ( 'NONE', #6271 ) ;
#8205 = LINE ( 'NONE', #7471, #8144 ) ;
#8206 = AXIS2_PLACEMENT_3D ( 'NONE', #485, #4783, #3484 ) ;
#8207 = EDGE_LOOP ( 'NONE', ( #3308, #1173, #9407, #691 ) ) ;
#8208 = CARTESIAN_POINT ( 'NONE',  ( -4.420886993428805312, 12.27057209469446875, 43.49964545912311564 ) ) ;
#8209 = EDGE_CURVE ( 'NONE', #3142, #2208, #1037, .T. ) ;
#8210 = DIRECTION ( 'NONE',  ( 1.000000000000000000, 0.000000000000000000, 0.000000000000000000 ) ) ;
#8211 = DIRECTION ( 'NONE',  ( -0.3286710990610907657, 0.000000000000000000, -0.9444444444444440867 ) ) ;
#8212 = AXIS2_PLACEMENT_3D ( 'NONE', #4424, #7386, #622 ) ;
#8213 = VERTEX_POINT ( 'NONE', #4219 ) ;
#8214 = CARTESIAN_POINT ( 'NONE',  ( 0.000000000000000000, 0.000000000000000000, 0.000000000000000000 ) ) ;
#8215 = ADVANCED_FACE ( 'NONE', ( #3419 ), #6417, .F. ) ;
#8216 = ORIENTED_EDGE ( 'NONE', *, *, #4693, .T. ) ;
#8217 = DIRECTION ( 'NONE',  ( -0.9860132971832694659, -1.788557213313974350E-28, 0.1666666666666658247 ) ) ;
#8218 = AXIS2_PLACEMENT_3D ( 'NONE', #6147, #7787, #7736 ) ;
#8219 = DIRECTION ( 'NONE',  ( 1.000000000000000000, 0.000000000000000000, 0.000000000000000000 ) ) ;
#8220 = DIRECTION ( 'NONE',  ( -1.000000000000000000, 0.000000000000000000, 0.000000000000000000 ) ) ;
#8221 = LINE ( 'NONE', #1701, #8126 ) ;
#8222 = DIRECTION ( 'NONE',  ( 0.000000000000000000, -1.000000000000000000, 0.000000000000000000 ) ) ;
#8223 = EDGE_LOOP ( 'NONE', ( #4736, #7874, #4420, #6167, #5803, #3060 ) ) ;
#8224 = EDGE_CURVE ( 'NONE', #6996, #8006, #5732, .T. ) ;
#8225 = CARTESIAN_POINT ( 'NONE',  ( 1.094544505994153880E-26, 56.50000000000029843, -26.00000000000002132 ) ) ;
#8226 = CARTESIAN_POINT ( 'NONE',  ( 9.737280834746197655, 0.9936006834773455365, 41.50515603427665923 ) ) ;
#8227 = CARTESIAN_POINT ( 'NONE',  ( -5.562309845534584518, 60.99999999999999289, 33.06426808735054124 ) ) ;
#8228 = VECTOR ( 'NONE', #4245, 1000.000000000000000 ) ;
#8229 = CARTESIAN_POINT ( 'NONE',  ( 0.000000000000000000, -50.91168824543140659, 0.000000000000000000 ) ) ;
#8230 = PLANE ( 'NONE',  #8152 ) ;
#8231 = LINE ( 'NONE', #5181, #4658 ) ;
#8232 = EDGE_CURVE ( 'NONE', #2716, #2421, #3459, .T. ) ;
#8233 = AXIS2_PLACEMENT_3D ( 'NONE', #3869, #9205, #9156 ) ;
#8234 = EDGE_CURVE ( 'NONE', #3142, #3425, #9344, .T. ) ;
#8235 = ADVANCED_FACE ( 'NONE', ( #4949 ), #8606, .F. ) ;
#8236 = CARTESIAN_POINT ( 'NONE',  ( 31.00000000000001066, 27.75862132583096553, -4.003261267919809185 ) ) ;
#8237 = DIRECTION ( 'NONE',  ( 0.5773502691896204020, -0.5773502691896366112, -0.5773502691896204020 ) ) ;
#8238 = ORIENTED_EDGE ( 'NONE', *, *, #916, .F. ) ;
#8239 = CARTESIAN_POINT ( 'NONE',  ( 9.762153702110021092E-27, 45.50000000000019185, -25.00000000000000000 ) ) ;
#8240 = DIRECTION ( 'NONE',  ( -1.735493991486225972E-29, 6.508102468073347395E-30, 1.000000000000000000 ) ) ;
#8241 = AXIS2_PLACEMENT_3D ( 'NONE', #6306, #1035, #4054 ) ;
#8242 = CIRCLE ( 'NONE', #6819, 27.00000000000000355 ) ;
#8243 = ORIENTED_EDGE ( 'NONE', *, *, #7816, .T. ) ;
#8244 = ADVANCED_FACE ( 'NONE', ( #1049 ), #361, .F. ) ;
#8245 = DIRECTION ( 'NONE',  ( -1.735493991486225972E-29, 6.508102468073347395E-30, 1.000000000000000000 ) ) ;
#8246 = DIRECTION ( 'NONE',  ( 1.000000000000000000, 0.000000000000000000, 0.000000000000000000 ) ) ;
#8247 = ORIENTED_EDGE ( 'NONE', *, *, #8799, .F. ) ;
#8248 = EDGE_CURVE ( 'NONE', #2204, #8074, #8011, .T. ) ;
#8249 = CIRCLE ( 'NONE', #9515, 40.00000000000000711 ) ;
#8250 = CARTESIAN_POINT ( 'NONE',  ( 13.18962522851849251, 5.248138163192250794, 36.70198719095098028 ) ) ;
#8251 = APPLICATION_PROTOCOL_DEFINITION ( 'draft international standard', 'automotive_design', 1998, #1394 ) ;
#8252 = VERTEX_POINT ( 'NONE', #4900 ) ;
#8253 = LINE ( 'NONE', #6907, #893 ) ;
#8254 = AXIS2_PLACEMENT_3D ( 'NONE', #5114, #7279, #1359 ) ;
#8255 = LINE ( 'NONE', #6075, #4819 ) ;
#8256 = ORIENTED_EDGE ( 'NONE', *, *, #8723, .T. ) ;
#8257 = LINE ( 'NONE', #4558, #1205 ) ;
#8258 = VERTEX_POINT ( 'NONE', #7914 ) ;
#8259 = CARTESIAN_POINT ( 'NONE',  ( 1.555535097482682654E-26, 78.08723716182652197, -25.00000000000000000 ) ) ;
#8260 = DIRECTION ( 'NONE',  ( -1.000000000000000000, 0.000000000000000000, -0.000000000000000000 ) ) ;
#8261 = EDGE_CURVE ( 'NONE', #3567, #7715, #9486, .T. ) ;
#8262 = DIRECTION ( 'NONE',  ( -0.3286710990610922090, -6.289316826390952918E-29, -0.9444444444444435316 ) ) ;
#8263 = ORIENTED_EDGE ( 'NONE', *, *, #5180, .F. ) ;
#8264 = CARTESIAN_POINT ( 'NONE',  ( 0.000000000000000000, 38.99999999999993605, 0.000000000000000000 ) ) ;
#8265 = FACE_OUTER_BOUND ( 'NONE', #8048, .T. ) ;
#8266 = VERTEX_POINT ( 'NONE', #1836 ) ;
#8267 = EDGE_CURVE ( 'NONE', #4918, #1718, #3313, .T. ) ;
#8268 = EDGE_LOOP ( 'NONE', ( #7349, #7536, #3, #2780 ) ) ;
#8269 = CARTESIAN_POINT ( 'NONE',  ( 6.000000000000001776, 29.14236109046821710, -29.24912810952613640 ) ) ;
#8270 = FACE_OUTER_BOUND ( 'NONE', #65, .T. ) ;
#8271 = DIRECTION ( 'NONE',  ( 0.000000000000000000, 1.000000000000000000, -0.000000000000000000 ) ) ;
#8272 = AXIS2_PLACEMENT_3D ( 'NONE', #5955, #8934, #1520 ) ;
#8273 = CIRCLE ( 'NONE', #7640, 2.499999999999998668 ) ;
#8274 = DIRECTION ( 'NONE',  ( 0.000000000000000000, 1.000000000000000000, 0.000000000000000000 ) ) ;
#8275 = CARTESIAN_POINT ( 'NONE',  ( -5.562309845534584518, 49.99999999999999289, 30.56426808735054124 ) ) ;
#8276 = CIRCLE ( 'NONE', #3065, 26.00000000000008171 ) ;
#8277 = ORIENTED_EDGE ( 'NONE', *, *, #51, .F. ) ;
#8278 = LINE ( 'NONE', #9661, #7501 ) ;
#8279 = CARTESIAN_POINT ( 'NONE',  ( 8.646527988035350276, -1.739381284455594923, 42.04573165431521176 ) ) ;
#8280 = CARTESIAN_POINT ( 'NONE',  ( 0.000000000000000000, 61.99999999999999289, 0.000000000000000000 ) ) ;
#8281 = CARTESIAN_POINT ( 'NONE',  ( -0.7306063396721927949, -15.00000000000000000, 30.53418880813659086 ) ) ;
#8282 = FACE_OUTER_BOUND ( 'NONE', #6054, .T. ) ;
#8283 = ORIENTED_EDGE ( 'NONE', *, *, #9140, .T. ) ;
#8284 = CARTESIAN_POINT ( 'NONE',  ( 6.000000000000007994, -10.00000000000000533, 26.32489316217636954 ) ) ;
#8285 = VECTOR ( 'NONE', #1689, 1000.000000000000000 ) ;
#8286 = VECTOR ( 'NONE', #8957, 1000.000000000000000 ) ;
#8287 = EDGE_CURVE ( 'NONE', #326, #6704, #5909, .T. ) ;
#8288 = VECTOR ( 'NONE', #5589, 1000.000000000000000 ) ;
#8289 = CONICAL_SURFACE ( 'NONE', #726, 17.99999999999999645, 0.7853981633974517207 ) ;
#8290 = ORIENTED_EDGE ( 'NONE', *, *, #7791, .T. ) ;
#8291 = PLANE ( 'NONE',  #3375 ) ;
#8292 = EDGE_CURVE ( 'NONE', #4231, #6362, #7498, .T. ) ;
#8293 = AXIS2_PLACEMENT_3D ( 'NONE', #7992, #4287, #491 ) ;
#8294 = VECTOR ( 'NONE', #8316, 1000.000000000000341 ) ;
#8295 = ORIENTED_EDGE ( 'NONE', *, *, #8118, .F. ) ;
#8296 = CARTESIAN_POINT ( 'NONE',  ( -23.54759692749571087, 39.99999999999999289, 18.58791755254458522 ) ) ;
#8297 = CARTESIAN_POINT ( 'NONE',  ( 1.945897168356747864, -15.00000000000000000, 30.21518419675670586 ) ) ;
#8298 = ORIENTED_EDGE ( 'NONE', *, *, #7390, .T. ) ;
#8299 = LINE ( 'NONE', #2250, #8722 ) ;
#8300 = VECTOR ( 'NONE', #2635, 1000.000000000000341 ) ;
#8301 = DIRECTION ( 'NONE',  ( 0.000000000000000000, 0.000000000000000000, -1.000000000000000000 ) ) ;
#8302 = ORIENTED_EDGE ( 'NONE', *, *, #4510, .T. ) ;
#8303 = CARTESIAN_POINT ( 'NONE',  ( 13.29364790190014212, 2.276109693707590420, 36.66440956898404124 ) ) ;
#8304 = DIRECTION ( 'NONE',  ( 1.000000000000000000, 0.000000000000000000, 0.000000000000000000 ) ) ;
#8305 = ORIENTED_EDGE ( 'NONE', *, *, #2240, .T. ) ;
#8306 = DIRECTION ( 'NONE',  ( -0.000000000000000000, 1.000000000000000000, -0.000000000000000000 ) ) ;
#8307 = EDGE_CURVE ( 'NONE', #7878, #6355, #697, .T. ) ;
#8308 = VECTOR ( 'NONE', #2052, 1000.000000000000000 ) ;
#8309 = DIRECTION ( 'NONE',  ( 0.000000000000000000, 0.000000000000000000, -1.000000000000000000 ) ) ;
#8310 = EDGE_CURVE ( 'NONE', #742, #294, #7659, .T. ) ;
#8311 = VERTEX_POINT ( 'NONE', #5042 ) ;
#8312 = CARTESIAN_POINT ( 'NONE',  ( -12.43339847825378719, 39.99999999999999289, 35.90836395996003461 ) ) ;
#8313 = EDGE_CURVE ( 'NONE', #1203, #5506, #6227, .T. ) ;
#8314 = ORIENTED_EDGE ( 'NONE', *, *, #9744, .T. ) ;
#8315 = CARTESIAN_POINT ( 'NONE',  ( -9.999999999999436895, 3.627100512255909681, 41.36423575989321222 ) ) ;
#8316 = DIRECTION ( 'NONE',  ( 0.9860132971832693549, 1.788557213313974126E-28, -0.1666666666666657970 ) ) ;
#8317 = DIRECTION ( 'NONE',  ( 0.000000000000000000, 0.000000000000000000, 1.000000000000000000 ) ) ;
#8318 = EDGE_LOOP ( 'NONE', ( #159, #195, #2621, #9101 ) ) ;
#8319 = LINE ( 'NONE', #1552, #262 ) ;
#8320 = LINE ( 'NONE', #2328, #7428 ) ;
#8321 = VERTEX_POINT ( 'NONE', #5091 ) ;
#8322 = UNCERTAINTY_MEASURE_WITH_UNIT (LENGTH_MEASURE( 1.000000000000000082E-05 ), #5849, 'distance_accuracy_value', 'NONE');
#8323 = ORIENTED_EDGE ( 'NONE', *, *, #5226, .T. ) ;
#8324 = CARTESIAN_POINT ( 'NONE',  ( 8.455602827837720289E-27, 41.50000000000020606, -24.09806918451538849 ) ) ;
#8325 = CARTESIAN_POINT ( 'NONE',  ( -0.6856205131675365827, -6.703820630692375993, 43.99932147620603473 ) ) ;
#8326 = DIRECTION ( 'NONE',  ( 0.5773502691896204020, 0.5773502691896363892, 0.5773502691896205130 ) ) ;
#8327 = DIRECTION ( 'NONE',  ( 0.000000000000000000, 0.000000000000000000, -1.000000000000000000 ) ) ;
#8328 = ORIENTED_EDGE ( 'NONE', *, *, #8070, .F. ) ;
#8329 = DIRECTION ( 'NONE',  ( -0.000000000000000000, -1.000000000000000000, -0.000000000000000000 ) ) ;
#8330 = VERTEX_POINT ( 'NONE', #8052 ) ;
#8331 = CARTESIAN_POINT ( 'NONE',  ( 33.06426808735054124, 60.99999999999999289, 5.562309845534586294 ) ) ;
#8332 = DIRECTION ( 'NONE',  ( -0.000000000000000000, -1.000000000000000000, -0.000000000000000000 ) ) ;
#8333 = LINE ( 'NONE', #5994, #5460 ) ;
#8334 = DIRECTION ( 'NONE',  ( -1.000000000000000000, 0.000000000000000000, 0.000000000000000000 ) ) ;
#8335 = FACE_OUTER_BOUND ( 'NONE', #4943, .T. ) ;
#8336 = CARTESIAN_POINT ( 'NONE',  ( 5.562309845534588959, 59.99999999999999289, -33.06426808735054124 ) ) ;
#8337 = ORIENTED_EDGE ( 'NONE', *, *, #9278, .F. ) ;
#8338 = FACE_OUTER_BOUND ( 'NONE', #449, .T. ) ;
#8339 = B_SPLINE_CURVE_WITH_KNOTS ( 'NONE', 3,
 ( #805, #4560, #1596, #3012, #9152, #4053 ),
 .UNSPECIFIED., .F., .F.,
 ( 4, 2, 4 ),
 ( 0.006018989108141225772, 0.009014550367373161052, 0.01201011162660509460 ),
 .UNSPECIFIED. ) ;
#8340 = DIRECTION ( 'NONE',  ( -0.000000000000000000, 0.000000000000000000, 1.000000000000000000 ) ) ;
#8341 = ORIENTED_EDGE ( 'NONE', *, *, #2249, .T. ) ;
#8342 = CARTESIAN_POINT ( 'NONE',  ( 31.11591804390324612, 61.99999999999999289, -4.904043666719942074 ) ) ;
#8343 = CARTESIAN_POINT ( 'NONE',  ( 3.810735843230694364, -15.00000000000000000, 29.48446022066782035 ) ) ;
#8344 = ORIENTED_EDGE ( 'NONE', *, *, #2488, .F. ) ;
#8345 = DIRECTION ( 'NONE',  ( 0.000000000000000000, 1.000000000000000000, 0.000000000000000000 ) ) ;
#8346 = CIRCLE ( 'NONE', #8254, 26.00000000000014566 ) ;
#8347 = DIRECTION ( 'NONE',  ( -0.000000000000000000, -0.000000000000000000, 1.000000000000000000 ) ) ;
#8348 = ORIENTED_EDGE ( 'NONE', *, *, #2239, .T. ) ;
#8349 = CARTESIAN_POINT ( 'NONE',  ( 12.94589496447643739, -0.1577490691376046139, 36.78875203023495999 ) ) ;
#8350 = APPLICATION_PROTOCOL_DEFINITION ( 'draft international standard', 'automotive_design', 1998, #5808 ) ;
#8351 = ORIENTED_EDGE ( 'NONE', *, *, #3833, .F. ) ;
#8352 = DIRECTION ( 'NONE',  ( -0.000000000000000000, 1.000000000000000000, -0.000000000000000000 ) ) ;
#8353 = LINE ( 'NONE', #1688, #6137 ) ;
#8354 = FACE_OUTER_BOUND ( 'NONE', #7627, .T. ) ;
#8355 = ORIENTED_EDGE ( 'NONE', *, *, #1108, .F. ) ;
#8356 = LINE ( 'NONE', #4614, #2449 ) ;
#8357 = ORIENTED_EDGE ( 'NONE', *, *, #6205, .T. ) ;
#8358 = CARTESIAN_POINT ( 'NONE',  ( -8.964960879312730668, 7.774309358726588570, 41.89665171198695504 ) ) ;
#8359 = AXIS2_PLACEMENT_3D ( 'NONE', #6844, #2489, #3092 ) ;
#8360 = AXIS2_PLACEMENT_3D ( 'NONE', #5314, #8917, #720 ) ;
#8361 = PRODUCT_DEFINITION_SHAPE ( 'NONE', 'NONE',  #9764 ) ;
#8362 = FACE_OUTER_BOUND ( 'NONE', #774, .T. ) ;
#8363 = DIRECTION ( 'NONE',  ( 0.000000000000000000, 0.000000000000000000, 1.000000000000000000 ) ) ;
#8364 = EDGE_CURVE ( 'NONE', #5147, #4621, #2284, .T. ) ;
#8365 = EDGE_CURVE ( 'NONE', #7381, #7113, #5236, .T. ) ;
#8366 = AXIS2_PLACEMENT_3D ( 'NONE', #6927, #3982, #7631 ) ;
#8367 = VERTEX_POINT ( 'NONE', #4305 ) ;
#8368 = CARTESIAN_POINT ( 'NONE',  ( -0.5436840601780645876, -9.469167920862840759, 39.52694059679008376 ) ) ;
#8369 = ORIENTED_EDGE ( 'NONE', *, *, #3189, .F. ) ;
#8370 = ORIENTED_EDGE ( 'NONE', *, *, #4260, .F. ) ;
#8371 = CARTESIAN_POINT ( 'NONE',  ( 1.300000000000000044, 3.252606517456513302E-16, 2.499999999999999556 ) ) ;
#8372 = DIRECTION ( 'NONE',  ( 0.000000000000000000, 0.000000000000000000, -1.000000000000000000 ) ) ;
#8373 = VECTOR ( 'NONE', #8818, 1000.000000000000000 ) ;
#8374 = CARTESIAN_POINT ( 'NONE',  ( 0.000000000000000000, 59.99999999999999289, 0.000000000000000000 ) ) ;
#8375 = EDGE_CURVE ( 'NONE', #2516, #4765, #4669, .T. ) ;
#8376 = ADVANCED_FACE ( 'NONE', ( #2763 ), #1431, .T. ) ;
#8377 = EDGE_LOOP ( 'NONE', ( #4613, #3931, #9504, #3615 ) ) ;
#8378 = CARTESIAN_POINT ( 'NONE',  ( -2.094888803305880518E-13, 59.99999999999999289, 30.00000000000000711 ) ) ;
#8379 = CARTESIAN_POINT ( 'NONE',  ( 0.000000000000000000, 61.99999999999999289, 0.000000000000000000 ) ) ;
#8380 = CARTESIAN_POINT ( 'NONE',  ( -3.976301758542435394, 59.47750853442943253, 35.00401529666655165 ) ) ;
#8381 = VERTEX_POINT ( 'NONE', #2900 ) ;
#8382 = CARTESIAN_POINT ( 'NONE',  ( 3.237977208914636140, -6.172201048711161597, 43.73371347798987330 ) ) ;
#8383 = CARTESIAN_POINT ( 'NONE',  ( 8.033901996508218346, 59.79149928942062786, -33.49300701350801290 ) ) ;
#8384 = DIRECTION ( 'NONE',  ( 0.000000000000000000, 0.000000000000000000, -1.000000000000000000 ) ) ;
#8385 = LINE ( 'NONE', #5518, #8685 ) ;
#8386 = ORIENTED_EDGE ( 'NONE', *, *, #4810, .T. ) ;
#8387 = CARTESIAN_POINT ( 'NONE',  ( 35.88888888888889284, 59.99999999999999289, -12.48950176432140502 ) ) ;
#8388 = CIRCLE ( 'NONE', #5545, 39.00000000000002132 ) ;
#8389 = ADVANCED_FACE ( 'NONE', ( #9424 ), #2637, .F. ) ;
#8390 = VECTOR ( 'NONE', #154, 1000.000000000000341 ) ;
#8391 = DIRECTION ( 'NONE',  ( -0.000000000000000000, -1.000000000000000000, -0.000000000000000000 ) ) ;
#8392 = EDGE_LOOP ( 'NONE', ( #8913, #4263, #9212, #2994 ) ) ;
#8393 = CARTESIAN_POINT ( 'NONE',  ( 5.562309845534588959, 60.99999999999999289, -33.06426808735054124 ) ) ;
#8394 = CARTESIAN_POINT ( 'NONE',  ( 5.490675478207040605, -15.00000000000000000, 28.78002780014356077 ) ) ;
#8395 = EDGE_CURVE ( 'NONE', #1760, #2374, #8762, .T. ) ;
#8396 = ORIENTED_EDGE ( 'NONE', *, *, #7182, .T. ) ;
#8397 = VECTOR ( 'NONE', #7913, 1000.000000000000000 ) ;
#8398 = LINE ( 'NONE', #3701, #3182 ) ;
#8399 = CARTESIAN_POINT ( 'NONE',  ( 0.000000000000000000, 59.99999999999999289, 0.000000000000000000 ) ) ;
#8400 = ORIENTED_EDGE ( 'NONE', *, *, #3630, .T. ) ;
#8401 = CARTESIAN_POINT ( 'NONE',  ( 10.00064848029234632, 3.603966413413724368, 41.36388302110313475 ) ) ;
#8402 = CIRCLE ( 'NONE', #8872, 34.49999999999999289 ) ;
#8403 = VERTEX_POINT ( 'NONE', #2109 ) ;
#8404 = CARTESIAN_POINT ( 'NONE',  ( 1.094544505994153880E-26, 55.00000000000030553, -24.09806918451524638 ) ) ;
#8405 = LINE ( 'NONE', #800, #8285 ) ;
#8406 = ORIENTED_EDGE ( 'NONE', *, *, #649, .T. ) ;
#8407 = CARTESIAN_POINT ( 'NONE',  ( -8.216777476527274970, 49.00000000000032685, -23.61111111111111427 ) ) ;
#8408 = VERTEX_POINT ( 'NONE', #3702 ) ;
#8409 = CARTESIAN_POINT ( 'NONE',  ( 9.318419442923201951E-27, 47.00000000000034106, -25.00000000000000000 ) ) ;
#8410 = AXIS2_PLACEMENT_3D ( 'NONE', #759, #3767, #9551 ) ;
#8411 = CARTESIAN_POINT ( 'NONE',  ( -4.104483837743832630, 61.95009619975343185, 37.32687308866060505 ) ) ;
#8412 = AXIS2_PLACEMENT_3D ( 'NONE', #2748, #3637, #5672 ) ;
#8413 = ADVANCED_FACE ( 'NONE', ( #2855 ), #5787, .T. ) ;
#8414 = VERTEX_POINT ( 'NONE', #5962 ) ;
#8415 = CARTESIAN_POINT ( 'NONE',  ( -6.397328100368723014, 58.99819947112212049, 35.43017184758411986 ) ) ;
#8416 = ORIENTED_EDGE ( 'NONE', *, *, #1780, .T. ) ;
#8417 = EDGE_LOOP ( 'NONE', ( #136, #1887, #8560, #4497, #2389 ) ) ;
#8418 = CARTESIAN_POINT ( 'NONE',  ( -0.5685535372354538763, -6.704273290862945878, 38.99985098249960913 ) ) ;
#8419 = ADVANCED_FACE ( 'NONE', ( #9732 ), #3876, .F. ) ;
#8420 = SURFACE_STYLE_USAGE ( .BOTH. , #233 ) ;
#8421 = CARTESIAN_POINT ( 'NONE',  ( 20.44670930779903983, 59.99999999999999289, 25.90235662024527841 ) ) ;
#8422 = ORIENTED_EDGE ( 'NONE', *, *, #3312, .F. ) ;
#8423 = DIRECTION ( 'NONE',  ( 0.000000000000000000, 0.000000000000000000, 1.000000000000000000 ) ) ;
#8424 = CARTESIAN_POINT ( 'NONE',  ( -35.88888888888889284, 39.99999999999999289, 12.48950176432140857 ) ) ;
#8425 = CARTESIAN_POINT ( 'NONE',  ( 2.284773941623177151, -6.446222133925260778, 43.86901922224630823 ) ) ;
#8426 = CARTESIAN_POINT ( 'NONE',  ( 7.123219286842092934, 59.18149658568249549, -35.02766888370167919 ) ) ;
#8427 = EDGE_CURVE ( 'NONE', #9075, #1923, #2157, .T. ) ;
#8428 = CARTESIAN_POINT ( 'NONE',  ( 1.084202172485504434E-15, 30.00000000000000000, 5.000000000000005329 ) ) ;
#8429 = CARTESIAN_POINT ( 'NONE',  ( 0.6684956564278037305, 18.29348733819152528, 38.99958749751832698 ) ) ;
#8430 = EDGE_CURVE ( 'NONE', #8583, #5461, #9676, .T. ) ;
#8431 = AXIS2_PLACEMENT_3D ( 'NONE', #3245, #9281, #545 ) ;
#8432 = DIRECTION ( 'NONE',  ( 0.000000000000000000, 0.000000000000000000, 1.000000000000000000 ) ) ;
#8433 = ORIENTED_EDGE ( 'NONE', *, *, #916, .T. ) ;
#8434 = CARTESIAN_POINT ( 'NONE',  ( 5.000000000000002665, 30.00000000000000000, -25.51470164434615029 ) ) ;
#8435 = AXIS2_PLACEMENT_3D ( 'NONE', #6624, #8961, #4277 ) ;
#8436 = VECTOR ( 'NONE', #8066, 1000.000000000000000 ) ;
#8437 = AXIS2_PLACEMENT_3D ( 'NONE', #7647, #4544, #3642 ) ;
#8438 = ORIENTED_EDGE ( 'NONE', *, *, #4743, .T. ) ;
#8439 = LINE ( 'NONE', #8493, #9369 ) ;
#8440 = PRODUCT_DEFINITION_SHAPE ( 'NONE', 'NONE',  #9755 ) ;
#8441 = ORIENTED_EDGE ( 'NONE', *, *, #8790, .T. ) ;
#8442 = CARTESIAN_POINT ( 'NONE',  ( 31.00000000000000711, -10.00000000000000533, 6.000000000000000000 ) ) ;
#8443 = DIRECTION ( 'NONE',  ( 0.000000000000000000, 0.000000000000000000, 1.000000000000000000 ) ) ;
#8444 = VERTEX_POINT ( 'NONE', #4404 ) ;
#8445 = AXIS2_PLACEMENT_3D ( 'NONE', #7252, #9530, #2103 ) ;
#8446 = AXIS2_PLACEMENT_3D ( 'NONE', #8174, #1405, #4332 ) ;
#8447 = CARTESIAN_POINT ( 'NONE',  ( 6.000000000000007994, 27.42469319230600533, 31.00000000000000711 ) ) ;
#8448 = CARTESIAN_POINT ( 'NONE',  ( 0.000000000000000000, 30.00000000000000000, -30.00000000000000711 ) ) ;
#8449 = ORIENTED_EDGE ( 'NONE', *, *, #7915, .F. ) ;
#8450 = AXIS2_PLACEMENT_3D ( 'NONE', #7709, #6803, #4653 ) ;
#8451 = VECTOR ( 'NONE', #3859, 1000.000000000000000 ) ;
#8452 = EDGE_CURVE ( 'NONE', #849, #7052, #5188, .T. ) ;
#8453 = CARTESIAN_POINT ( 'NONE',  ( 4.270857271783432552, -10.91876588853619445, 38.76773248714805931 ) ) ;
#8454 = VECTOR ( 'NONE', #2568, 1000.000000000000000 ) ;
#8455 = ITEM_DEFINED_TRANSFORMATION ( 'NONE', 'NONE', #5392,  #6314 ) ;
#8456 = VECTOR ( 'NONE', #9716, 1000.000000000000000 ) ;
#8457 = AXIS2_PLACEMENT_3D ( 'NONE', #1060, #4128, #9307 ) ;
#8458 = CARTESIAN_POINT ( 'NONE',  ( 33.06426808735054124, 49.99999999999999289, 5.562309845534586294 ) ) ;
#8459 = CARTESIAN_POINT ( 'NONE',  ( 4.837354856632047030E-15, 30.00000000000000000, -39.00000000000002132 ) ) ;
#8460 = LINE ( 'NONE', #9339, #7844 ) ;
#8461 = ORIENTED_EDGE ( 'NONE', *, *, #4068, .T. ) ;
#8462 = AXIS2_PLACEMENT_3D ( 'NONE', #2027, #9361, #5613 ) ;
#8463 = CIRCLE ( 'NONE', #7826, 1.500000000000000888 ) ;
#8464 = PLANE ( 'NONE',  #984 ) ;
#8465 = CARTESIAN_POINT ( 'NONE',  ( 26.32489316217636954, 30.00000000000000000, -6.000000000000006217 ) ) ;
#8466 = PRESENTATION_LAYER_ASSIGNMENT (  '', '', ( #3416 ) ) ;
#8467 =( REPRESENTATION_RELATIONSHIP ('NONE','NONE', #5841, #490 ) REPRESENTATION_RELATIONSHIP_WITH_TRANSFORMATION ( #3914 )SHAPE_REPRESENTATION_RELATIONSHIP( ) );
#8468 = ORIENTED_EDGE ( 'NONE', *, *, #7446, .T. ) ;
#8469 = CARTESIAN_POINT ( 'NONE',  ( -8.033901996508213017, 59.79149928942061365, 33.49300701350799159 ) ) ;
#8470 = ORIENTED_EDGE ( 'NONE', *, *, #6475, .F. ) ;
#8471 = ORIENTED_EDGE ( 'NONE', *, *, #7457, .F. ) ;
#8472 = CARTESIAN_POINT ( 'NONE',  ( 1.300000000000000044, 0.7216878364870328300, -1.250000000000000000 ) ) ;
#8473 = SURFACE_STYLE_FILL_AREA ( #3173 ) ;
#8474 = LINE ( 'NONE', #4773, #2721 ) ;
#8475 = AXIS2_PLACEMENT_3D ( 'NONE', #9662, #2790, #8034 ) ;
#8476 = EDGE_CURVE ( 'NONE', #8999, #8611, #7258, .T. ) ;
#8477 = VERTEX_POINT ( 'NONE', #8843 ) ;
#8478 = DIRECTION ( 'NONE',  ( -1.820952055660014662E-28, -1.000000000000000000, -7.038118388768679669E-30 ) ) ;
#8479 = DIRECTION ( 'NONE',  ( -0.000000000000000000, -0.5000000000000001110, -0.8660254037844385966 ) ) ;
#8480 = ORIENTED_EDGE ( 'NONE', *, *, #1515, .F. ) ;
#8481 = LINE ( 'NONE', #7784, #2526 ) ;
#8482 = CARTESIAN_POINT ( 'NONE',  ( 7.766845228004612522, 59.52671121465669302, -34.26018231648108525 ) ) ;
#8483 = DIRECTION ( 'NONE',  ( -1.000000000000000000, -0.000000000000000000, -0.000000000000000000 ) ) ;
#8484 = SURFACE_STYLE_USAGE ( .BOTH. , #7639 ) ;
#8485 = CARTESIAN_POINT ( 'NONE',  ( -31.00000000000000711, -10.00000000000000533, 6.000000000000009770 ) ) ;
#8486 = ORIENTED_EDGE ( 'NONE', *, *, #4014, .T. ) ;
#8487 = DIRECTION ( 'NONE',  ( -1.776356839400250465E-15, 0.000000000000000000, 1.000000000000000000 ) ) ;
#8488 = ADVANCED_FACE ( 'NONE', ( #7413 ), #3504, .T. ) ;
#8489 = EDGE_CURVE ( 'NONE', #7928, #6799, #519, .T. ) ;
#8490 = EDGE_CURVE ( 'NONE', #5790, #1519, #3209, .T. ) ;
#8491 = DIRECTION ( 'NONE',  ( -1.000000000000000000, -0.000000000000000000, -0.000000000000000000 ) ) ;
#8492 = DIRECTION ( 'NONE',  ( 0.000000000000000000, 0.000000000000000000, 1.000000000000000000 ) ) ;
#8493 = CARTESIAN_POINT ( 'NONE',  ( 4.000000000000002665, 28.99999999999997158, -8.673617379884032514E-16 ) ) ;
#8494 = ORIENTED_EDGE ( 'NONE', *, *, #2997, .F. ) ;
#8495 = CARTESIAN_POINT ( 'NONE',  ( 8.871504613779926274, 62.00000000000265743, -36.13240710991932048 ) ) ;
#8496 = CARTESIAN_POINT ( 'NONE',  ( 36.64076086657617282, 61.94822636785970360, 8.307112375470062204 ) ) ;
#8497 = ORIENTED_EDGE ( 'NONE', *, *, #5087, .F. ) ;
#8498 = PLANE ( 'NONE',  #4779 ) ;
#8499 = CARTESIAN_POINT ( 'NONE',  ( -35.86802812777743554, 61.99999999999999289, -9.082100980773358145 ) ) ;
#8500 = ORIENTED_EDGE ( 'NONE', *, *, #3274, .F. ) ;
#8501 = CARTESIAN_POINT ( 'NONE',  ( -5.562309845534584518, 59.99999999999999289, 33.06426808735054124 ) ) ;
#8502 = EDGE_CURVE ( 'NONE', #2405, #8204, #6550, .T. ) ;
#8503 = FACE_OUTER_BOUND ( 'NONE', #1680, .T. ) ;
#8504 = ORIENTED_EDGE ( 'NONE', *, *, #1947, .T. ) ;
#8505 = DIRECTION ( 'NONE',  ( 0.000000000000000000, 0.000000000000000000, 1.000000000000000000 ) ) ;
#8506 = DIRECTION ( 'NONE',  ( 0.000000000000000000, 1.000000000000000000, 0.000000000000000000 ) ) ;
#8507 = VERTEX_POINT ( 'NONE', #119 ) ;
#8508 = CARTESIAN_POINT ( 'NONE',  ( 9.815840903884561541, 59.99999999999999289, -28.34870838944214100 ) ) ;
#8509 = CARTESIAN_POINT ( 'NONE',  ( -5.861437416230651287, -4.813697954704956317, 43.11457445622953344 ) ) ;
#8510 = VERTEX_POINT ( 'NONE', #6902 ) ;
#8511 = CARTESIAN_POINT ( 'NONE',  ( -34.57348461147494589, 59.39325349372419538, -7.561715963717763778 ) ) ;
#8512 = EDGE_CURVE ( 'NONE', #269, #7542, #3199, .T. ) ;
#8513 = EDGE_LOOP ( 'NONE', ( #8599, #1562, #2700, #3361 ) ) ;
#8514 = DIRECTION ( 'NONE',  ( 0.000000000000000000, 0.000000000000000000, 1.000000000000000000 ) ) ;
#8515 = VECTOR ( 'NONE', #6779, 1000.000000000000000 ) ;
#8516 = VECTOR ( 'NONE', #4004, 1000.000000000000000 ) ;
#8517 = ORIENTED_EDGE ( 'NONE', *, *, #9122, .F. ) ;
#8518 = CARTESIAN_POINT ( 'NONE',  ( -13.29668680294569683, 2.328753113016122533, 36.66330756792502399 ) ) ;
#8519 = LINE ( 'NONE', #2382, #4631 ) ;
#8520 = EDGE_CURVE ( 'NONE', #5750, #1595, #6209, .T. ) ;
#8521 = CIRCLE ( 'NONE', #4419, 2.500000000000002220 ) ;
#8522 = EDGE_LOOP ( 'NONE', ( #4554, #91 ) ) ;
#8523 = CARTESIAN_POINT ( 'NONE',  ( 0.000000000000000000, 0.000000000000000000, 0.000000000000000000 ) ) ;
#8524 = ORIENTED_EDGE ( 'NONE', *, *, #7223, .F. ) ;
#8525 = FACE_OUTER_BOUND ( 'NONE', #1797, .T. ) ;
#8526 = DIRECTION ( 'NONE',  ( -0.000000000000000000, 1.000000000000000000, -0.000000000000000000 ) ) ;
#8527 = FACE_OUTER_BOUND ( 'NONE', #7144, .T. ) ;
#8528 = DIRECTION ( 'NONE',  ( -0.3286710990610922090, -6.289316826390952918E-29, -0.9444444444444435316 ) ) ;
#8529 = LINE ( 'NONE', #6252, #7655 ) ;
#8530 = AXIS2_PLACEMENT_3D ( 'NONE', #5375, #4087, #2342 ) ;
#8531 = ADVANCED_FACE ( 'NONE', ( #9142 ), #576, .T. ) ;
#8532 = EDGE_CURVE ( 'NONE', #577, #9341, #4834, .T. ) ;
#8533 = CYLINDRICAL_SURFACE ( 'NONE', #4962, 27.00000000000000355 ) ;
#8534 = ORIENTED_EDGE ( 'NONE', *, *, #1012, .F. ) ;
#8535 = CARTESIAN_POINT ( 'NONE',  ( 7.819489076939989403, 61.89591950820473443, -36.97167050927863130 ) ) ;
#8536 = CARTESIAN_POINT ( 'NONE',  ( 0.000000000000000000, 58.99999999999999289, -37.00000000000000711 ) ) ;
#8537 = ORIENTED_EDGE ( 'NONE', *, *, #8452, .T. ) ;
#8538 = EDGE_CURVE ( 'NONE', #6892, #8403, #2915, .T. ) ;
#8539 = DIRECTION ( 'NONE',  ( -0.000000000000000000, -1.000000000000000000, -0.000000000000000000 ) ) ;
#8540 = B_SPLINE_CURVE_WITH_KNOTS ( 'NONE', 3,
 ( #7892, #7136, #3387, #539 ),
 .UNSPECIFIED., .F., .F.,
 ( 4, 4 ),
 ( 9.813077866773594792E-18, 0.003679109433542027217 ),
 .UNSPECIFIED. ) ;
#8541 = EDGE_CURVE ( 'NONE', #1776, #5052, #1814, .T. ) ;
#8542 = CARTESIAN_POINT ( 'NONE',  ( 1.820000000000000062, 3.799999999999999378, 0.000000000000000000 ) ) ;
#8543 = DIRECTION ( 'NONE',  ( 0.9860132971832693549, 1.788557213313974126E-28, -0.1666666666666657970 ) ) ;
#8544 = EDGE_CURVE ( 'NONE', #3167, #7710, #7339, .T. ) ;
#8545 = CARTESIAN_POINT ( 'NONE',  ( 3.852137862560303105, -5.973899105776613538, 38.86704162447477273 ) ) ;
#8546 = ORIENTED_EDGE ( 'NONE', *, *, #7704, .T. ) ;
#8547 = CYLINDRICAL_SURFACE ( 'NONE', #85, 31.49999999999999289 ) ;
#8548 = ADVANCED_FACE ( 'NONE', ( #4550 ), #1475, .F. ) ;
#8549 = ORIENTED_EDGE ( 'NONE', *, *, #1061, .F. ) ;
#8550 = LINE ( 'NONE', #4754, #1809 ) ;
#8551 = ORIENTED_EDGE ( 'NONE', *, *, #7022, .T. ) ;
#8552 = DIRECTION ( 'NONE',  ( -0.000000000000000000, 1.000000000000000000, -0.000000000000000000 ) ) ;
#8553 = VECTOR ( 'NONE', #4403, 1000.000000000000341 ) ;
#8554 = VERTEX_POINT ( 'NONE', #4500 ) ;
#8555 = EDGE_CURVE ( 'NONE', #8403, #7011, #8, .T. ) ;
#8556 = EDGE_CURVE ( 'NONE', #7590, #1536, #7657, .T. ) ;
#8557 = EDGE_CURVE ( 'NONE', #156, #1097, #3912, .T. ) ;
#8558 = FACE_OUTER_BOUND ( 'NONE', #2274, .T. ) ;
#8559 = DIRECTION ( 'NONE',  ( 0.000000000000000000, 0.000000000000000000, -1.000000000000000000 ) ) ;
#8560 = ORIENTED_EDGE ( 'NONE', *, *, #1418, .F. ) ;
#8561 = LINE ( 'NONE', #6963, #4044 ) ;
#8562 = VERTEX_POINT ( 'NONE', #3149 ) ;
#8563 = LINE ( 'NONE', #2515, #8454 ) ;
#8564 = ORIENTED_EDGE ( 'NONE', *, *, #4694, .T. ) ;
#8565 = CARTESIAN_POINT ( 'NONE',  ( -9.120756353288166807, -7.629869846859943294, 37.91977750705790129 ) ) ;
#8566 = VECTOR ( 'NONE', #4821, 1000.000000000000000 ) ;
#8567 = CARTESIAN_POINT ( 'NONE',  ( 8.673617379884035472E-16, -1.899999999999999689, -3.490243377569955075E-16 ) ) ;
#8568 = CARTESIAN_POINT ( 'NONE',  ( -3.153634179030417872, 61.99999999999999289, 36.86535760663188199 ) ) ;
#8569 = AXIS2_PLACEMENT_3D ( 'NONE', #5179, #5129, #9665 ) ;
#8570 = EDGE_CURVE ( 'NONE', #1789, #909, #5439, .T. ) ;
#8571 = ORIENTED_EDGE ( 'NONE', *, *, #9204, .T. ) ;
#8572 = LINE ( 'NONE', #1751, #7576 ) ;
#8573 = ORIENTED_EDGE ( 'NONE', *, *, #468, .F. ) ;
#8574 = LINE ( 'NONE', #1801, #1172 ) ;
#8575 = DIRECTION ( 'NONE',  ( 0.000000000000000000, 0.000000000000000000, 1.000000000000000000 ) ) ;
#8576 = CARTESIAN_POINT ( 'NONE',  ( 0.000000000000000000, 59.99999999999999289, 0.000000000000000000 ) ) ;
#8577 = DIRECTION ( 'NONE',  ( -1.000000000000000000, 0.000000000000000000, 0.000000000000000000 ) ) ;
#8578 = FACE_OUTER_BOUND ( 'NONE', #5549, .T. ) ;
#8579 = CARTESIAN_POINT ( 'NONE',  ( 6.000000000000001776, -10.00000000000000533, -31.00000000000000711 ) ) ;
#8580 = VERTEX_POINT ( 'NONE', #4703 ) ;
#8581 = AXIS2_PLACEMENT_3D ( 'NONE', #5570, #5430, #4697 ) ;
#8582 = CARTESIAN_POINT ( 'NONE',  ( 0.000000000000000000, -15.00000000000000000, 0.000000000000000000 ) ) ;
#8583 = VERTEX_POINT ( 'NONE', #940 ) ;
#8584 = CARTESIAN_POINT ( 'NONE',  ( 6.890850105526419966, 61.82663791069490600, -37.37679511928140386 ) ) ;
#8585 = DIRECTION ( 'NONE',  ( 1.820952055660014662E-28, 1.000000000000000000, 7.038118388768679669E-30 ) ) ;
#8586 = ORIENTED_EDGE ( 'NONE', *, *, #1788, .F. ) ;
#8587 = CARTESIAN_POINT ( 'NONE',  ( -3.246812748820610661, 12.77555213868837569, 43.73912123486446291 ) ) ;
#8588 = ADVANCED_FACE ( 'NONE', ( #3953 ), #1195, .T. ) ;
#8589 = FACE_OUTER_BOUND ( 'NONE', #1395, .T. ) ;
#8590 = AXIS2_PLACEMENT_3D ( 'NONE', #6555, #452, #7859 ) ;
#8591 = CONICAL_SURFACE ( 'NONE', #1805, 40.00000000000000711, 0.7853981633974482790 ) ;
#8592 = CARTESIAN_POINT ( 'NONE',  ( 6.000000000000007994, -10.00000000000000533, 31.00000000000000711 ) ) ;
#8593 = CARTESIAN_POINT ( 'NONE',  ( 5.225835130983021770, -5.267432217960810625, 38.73366001166045436 ) ) ;
#8594 = CARTESIAN_POINT ( 'NONE',  ( -28.37252191822215863, 30.00000000000000000, 6.000000000000009770 ) ) ;
#8595 = AXIS2_PLACEMENT_3D ( 'NONE', #7051, #1734, #7106 ) ;
#8596 = CIRCLE ( 'NONE', #9385, 28.99999999999995026 ) ;
#8597 = VERTEX_POINT ( 'NONE', #3753 ) ;
#8598 = CARTESIAN_POINT ( 'NONE',  ( 23.54469556655648077, 39.99999999999999289, 29.82695610816123022 ) ) ;
#8599 = ORIENTED_EDGE ( 'NONE', *, *, #1714, .F. ) ;
#8600 = CARTESIAN_POINT ( 'NONE',  ( 0.9994180975881575835, 27.99999999999992184, 31.00000000000001066 ) ) ;
#8601 = ORIENTED_EDGE ( 'NONE', *, *, #4604, .F. ) ;
#8602 = PRODUCT ( 'Lever with a Die for Securing the Metal Body', 'Lever with a Die for Securing the Metal Body', '', ( #4504 ) ) ;
#8603 = LINE ( 'NONE', #9445, #3985 ) ;
#8604 = VECTOR ( 'NONE', #3855, 1000.000000000000000 ) ;
#8605 = CIRCLE ( 'NONE', #3878, 30.00000000000000711 ) ;
#8606 = PLANE ( 'NONE',  #7013 ) ;
#8607 = VECTOR ( 'NONE', #6327, 1000.000000000000000 ) ;
#8608 = AXIS2_PLACEMENT_3D ( 'NONE', #4574, #3075, #182 ) ;
#8609 = EDGE_CURVE ( 'NONE', #1828, #4609, #1084, .T. ) ;
#8610 = EDGE_CURVE ( 'NONE', #9714, #8999, #2604, .T. ) ;
#8611 = VERTEX_POINT ( 'NONE', #7151 ) ;
#8612 = ORIENTED_EDGE ( 'NONE', *, *, #748, .F. ) ;
#8613 = CARTESIAN_POINT ( 'NONE',  ( 3.153634179030674556, 61.99999999999999289, -36.86535760663186068 ) ) ;
#8614 = EDGE_CURVE ( 'NONE', #4883, #4501, #5777, .T. ) ;
#8615 = AXIS2_PLACEMENT_3D ( 'NONE', #6019, #6715, #6910 ) ;
#8616 = ORIENTED_EDGE ( 'NONE', *, *, #7237, .F. ) ;
#8617 = ORIENTED_EDGE ( 'NONE', *, *, #3530, .T. ) ;
#8618 = CARTESIAN_POINT ( 'NONE',  ( 1.820000000000000062, -3.800000000000000266, -4.653657836759940757E-16 ) ) ;
#8619 = ORIENTED_EDGE ( 'NONE', *, *, #8232, .F. ) ;
#8620 = CIRCLE ( 'NONE', #6081, 2.500000000000002220 ) ;
#8621 = VERTEX_POINT ( 'NONE', #1726 ) ;
#8622 = CIRCLE ( 'NONE', #6868, 37.00000000000000711 ) ;
#8623 = CARTESIAN_POINT ( 'NONE',  ( -5.854220575332682586, -4.818998781743923487, 43.11681015548058582 ) ) ;
#8624 = DIRECTION ( 'NONE',  ( 0.000000000000000000, 0.000000000000000000, 1.000000000000000000 ) ) ;
#8625 = FACE_OUTER_BOUND ( 'NONE', #5123, .T. ) ;
#8626 = AXIS2_PLACEMENT_3D ( 'NONE', #5027, #3447, #8785 ) ;
#8627 = CLOSED_SHELL ( 'NONE', ( #2403, #5191, #3900, #9627, #4892, #4874, #5760, #34, #4989, #6788, #8376, #6705, #4009, #8419, #4628, #5040, #3526, #2523, #7036, #5109, #1965, #5471, #7810, #5273, #7833, #6367, #4142 ) ) ;
#8628 = ORIENTED_EDGE ( 'NONE', *, *, #9093, .T. ) ;
#8629 = DIRECTION ( 'NONE',  ( 0.9860132971832693549, 1.788557213313974126E-28, -0.1666666666666657970 ) ) ;
#8630 = ORIENTED_EDGE ( 'NONE', *, *, #2451, .T. ) ;
#8631 = CARTESIAN_POINT ( 'NONE',  ( 26.32489316217636954, -10.00000000000000533, -6.000000000000006217 ) ) ;
#8632 = CARTESIAN_POINT ( 'NONE',  ( -6.000000000000005329, -15.00000000000000000, -26.32489316217636954 ) ) ;
#8633 = CARTESIAN_POINT ( 'NONE',  ( 0.000000000000000000, 30.00000000000000000, 0.000000000000000000 ) ) ;
#8634 = CARTESIAN_POINT ( 'NONE',  ( 5.371095444502685723, 60.99999999999999289, 34.07933880998929510 ) ) ;
#8635 = CARTESIAN_POINT ( 'NONE',  ( 0.000000000000000000, 39.99999999999999289, 0.000000000000000000 ) ) ;
#8636 = DIRECTION ( 'NONE',  ( -0.1666666666666658525, -3.897465909857536228E-29, -0.9860132971832695770 ) ) ;
#8637 = ORIENTED_EDGE ( 'NONE', *, *, #2983, .T. ) ;
#8638 = LINE ( 'NONE', #9322, #3854 ) ;
#8639 = ORIENTED_EDGE ( 'NONE', *, *, #3236, .F. ) ;
#8640 = PLANE ( 'NONE',  #4306 ) ;
#8641 = LINE ( 'NONE', #5488, #5152 ) ;
#8642 = EDGE_LOOP ( 'NONE', ( #9109, #8850, #3158, #1531 ) ) ;
#8643 = FACE_OUTER_BOUND ( 'NONE', #8026, .T. ) ;
#8644 = DIRECTION ( 'NONE',  ( 1.000000000000000000, 0.000000000000000000, 0.000000000000000000 ) ) ;
#8645 = LINE ( 'NONE', #1867, #6558 ) ;
#8646 = CARTESIAN_POINT ( 'NONE',  ( 6.587360613405085275, -4.236025479845884512, 42.87792995678174890 ) ) ;
#8647 = DIRECTION ( 'NONE',  ( -0.3286710990610922090, -6.289316826390952918E-29, -0.9444444444444435316 ) ) ;
#8648 = ORIENTED_EDGE ( 'NONE', *, *, #4021, .F. ) ;
#8649 = CARTESIAN_POINT ( 'NONE',  ( -4.000000000000005329, 30.00000000000000000, -24.67792535850613334 ) ) ;
#8650 = CARTESIAN_POINT ( 'NONE',  ( 1.300000000000000044, 1.443375672974065216, 1.084202172492522584E-16 ) ) ;
#8651 = ORIENTED_EDGE ( 'NONE', *, *, #1407, .F. ) ;
#8652 = APPLICATION_CONTEXT ( 'automotive_design' ) ;
#8653 = CARTESIAN_POINT ( 'NONE',  ( -5.562309845534701758, 60.99999999999999289, 33.06426808735052703 ) ) ;
#8654 = CARTESIAN_POINT ( 'NONE',  ( 0.000000000000000000, 30.00000000000000000, 0.000000000000000000 ) ) ;
#8655 = UNCERTAINTY_MEASURE_WITH_UNIT (LENGTH_MEASURE( 1.000000000000000082E-05 ), #6806, 'distance_accuracy_value', 'NONE');
#8656 = CARTESIAN_POINT ( 'NONE',  ( -5.562309845534588071, 63.19999999999998153, 33.06426808735054124 ) ) ;
#8657 = ORIENTED_EDGE ( 'NONE', *, *, #5906, .F. ) ;
#8658 = DIRECTION ( 'NONE',  ( -0.000000000000000000, -0.000000000000000000, 1.000000000000000000 ) ) ;
#8659 = VERTEX_POINT ( 'NONE', #3298 ) ;
#8660 = ORIENTED_EDGE ( 'NONE', *, *, #2674, .T. ) ;
#8661 = CARTESIAN_POINT ( 'NONE',  ( 0.000000000000000000, 0.000000000000000000, 0.000000000000000000 ) ) ;
#8662 = ORIENTED_EDGE ( 'NONE', *, *, #3441, .F. ) ;
#8663 = ORIENTED_EDGE ( 'NONE', *, *, #7254, .F. ) ;
#8664 = CARTESIAN_POINT ( 'NONE',  ( -7.533180272099675001, -3.289707944753238245, 42.52548976219601684 ) ) ;
#8665 = EDGE_CURVE ( 'NONE', #5592, #5397, #5632, .T. ) ;
#8666 = EDGE_CURVE ( 'NONE', #1639, #8204, #5934, .T. ) ;
#8667 = CARTESIAN_POINT ( 'NONE',  ( -8.545448575588407536, -1.821351948407008946E-27, -24.55555555555568148 ) ) ;
#8668 = EDGE_CURVE ( 'NONE', #2914, #1527, #3251, .T. ) ;
#8669 = AXIS2_PLACEMENT_3D ( 'NONE', #1167, #442, #9467 ) ;
#8670 = ORIENTED_EDGE ( 'NONE', *, *, #9582, .T. ) ;
#8671 = CARTESIAN_POINT ( 'NONE',  ( 12.48950176432140680, 39.99999999999999289, 35.88888888888889284 ) ) ;
#8672 = ORIENTED_EDGE ( 'NONE', *, *, #6641, .F. ) ;
#8673 = CYLINDRICAL_SURFACE ( 'NONE', #2846, 26.00000000000011369 ) ;
#8674 = CYLINDRICAL_SURFACE ( 'NONE', #8462, 26.00000000000014566 ) ;
#8675 = DIRECTION ( 'NONE',  ( -0.000000000000000000, -1.000000000000000000, -0.000000000000000000 ) ) ;
#8676 = CARTESIAN_POINT ( 'NONE',  ( 9.780907758090382487, 13.46073421343169052, 37.75414574899522790 ) ) ;
#8677 = DIRECTION ( 'NONE',  ( -1.000000000000000000, 0.000000000000000000, -0.000000000000000000 ) ) ;
#8678 = EDGE_CURVE ( 'NONE', #2267, #1008, #6359, .T. ) ;
#8679 = CARTESIAN_POINT ( 'NONE',  ( 0.000000000000000000, 61.99999999999999289, 0.000000000000000000 ) ) ;
#8680 = AXIS2_PLACEMENT_3D ( 'NONE', #3534, #3390, #8778 ) ;
#8681 = AXIS2_PLACEMENT_3D ( 'NONE', #9243, #9381, #2606 ) ;
#8682 = EDGE_CURVE ( 'NONE', #8947, #6014, #6397, .T. ) ;
#8683 = VERTEX_POINT ( 'NONE', #6308 ) ;
#8684 = CARTESIAN_POINT ( 'NONE',  ( 30.00000000000000711, 59.99999999999999289, 1.047444401652940259E-13 ) ) ;
#8685 = VECTOR ( 'NONE', #8528, 1000.000000000000000 ) ;
#8686 = LINE ( 'NONE', #1909, #6994 ) ;
#8687 = PRODUCT_DEFINITION_SHAPE ( 'NONE', 'NONE',  #850 ) ;
#8688 = VERTEX_POINT ( 'NONE', #7749 ) ;
#8689 = CARTESIAN_POINT ( 'NONE',  ( -35.90836395996003461, 54.99999999999999289, -12.43339847825377475 ) ) ;
#8690 = PLANE ( 'NONE',  #4368 ) ;
#8691 = EDGE_LOOP ( 'NONE', ( #611, #7601, #7455, #8874 ) ) ;
#8692 = DIRECTION ( 'NONE',  ( 0.000000000000000000, 0.000000000000000000, -1.000000000000000000 ) ) ;
#8693 = CARTESIAN_POINT ( 'NONE',  ( 4.653657836759942730E-15, 59.99999999999999289, -38.00000000000000711 ) ) ;
#8694 = CONICAL_SURFACE ( 'NONE', #4274, 40.00000000000000711, 0.7853981633974482790 ) ;
#8695 = CARTESIAN_POINT ( 'NONE',  ( -30.00000000000001066, 59.99999999999999289, -3.252551416882082410E-13 ) ) ;
#8696 = EDGE_CURVE ( 'NONE', #9233, #1864, #986, .T. ) ;
#8697 = COLOUR_RGB ( '',0.7921568627450980005, 0.8196078431372548767, 0.9333333333333333481 ) ;
#8698 = VERTEX_POINT ( 'NONE', #7802 ) ;
#8699 = CARTESIAN_POINT ( 'NONE',  ( -31.16666666666674601, 59.99999999999999289, 10.84614626901577772 ) ) ;
#8700 = CARTESIAN_POINT ( 'NONE',  ( -5.552440503301123265, -15.00000000000030909, 36.79988656443232742 ) ) ;
#8701 = ORIENTED_EDGE ( 'NONE', *, *, #8520, .T. ) ;
#8702 = DIRECTION ( 'NONE',  ( 0.3286710990610922090, 6.289316826390952918E-29, 0.9444444444444435316 ) ) ;
#8703 = AXIS2_PLACEMENT_3D ( 'NONE', #2767, #2021, #606 ) ;
#8704 = CARTESIAN_POINT ( 'NONE',  ( 1.109999172770812503, 13.23925573637847997, 38.99045641393601613 ) ) ;
#8705 = CARTESIAN_POINT ( 'NONE',  ( 0.000000000000000000, 0.000000000000000000, 0.000000000000000000 ) ) ;
#8706 = VECTOR ( 'NONE', #3788, 1000.000000000000000 ) ;
#8707 = EDGE_LOOP ( 'NONE', ( #6442, #3664 ) ) ;
#8708 = CYLINDRICAL_SURFACE ( 'NONE', #9083, 38.00000000000000711 ) ;
#8709 = ORIENTED_EDGE ( 'NONE', *, *, #6332, .T. ) ;
#8710 = FACE_OUTER_BOUND ( 'NONE', #4193, .T. ) ;
#8711 = ORIENTED_EDGE ( 'NONE', *, *, #2116, .T. ) ;
#8712 = CARTESIAN_POINT ( 'NONE',  ( -8.387767640013615633, -2.225892194537749447, 38.23251940671359250 ) ) ;
#8713 = CARTESIAN_POINT ( 'NONE',  ( -33.00000000000000711, 59.99999999999999289, -3.456566525454702653E-13 ) ) ;
#8714 = EDGE_CURVE ( 'NONE', #6748, #4852, #7672, .T. ) ;
#8715 = AXIS2_PLACEMENT_3D ( 'NONE', #1597, #758, #910 ) ;
#8716 = FACE_OUTER_BOUND ( 'NONE', #3644, .T. ) ;
#8717 = ORIENTED_EDGE ( 'NONE', *, *, #1000, .F. ) ;
#8718 = FACE_OUTER_BOUND ( 'NONE', #3863, .T. ) ;
#8719 = EDGE_CURVE ( 'NONE', #8510, #1467, #8645, .T. ) ;
#8720 = EDGE_LOOP ( 'NONE', ( #456, #6329, #1078, #9309 ) ) ;
#8721 = DIRECTION ( 'NONE',  ( 0.000000000000000000, 0.000000000000000000, 1.000000000000000000 ) ) ;
#8722 = VECTOR ( 'NONE', #5436, 1000.000000000000000 ) ;
#8723 = EDGE_CURVE ( 'NONE', #4855, #8890, #4638, .T. ) ;
#8724 = CARTESIAN_POINT ( 'NONE',  ( 0.000000000000000000, 52.29648987751954792, 0.000000000000000000 ) ) ;
#8725 = CARTESIAN_POINT ( 'NONE',  ( 12.92792341719169791, 6.856606603030884983, 36.79514769918270645 ) ) ;
#8726 = DIRECTION ( 'NONE',  ( 0.000000000000000000, 0.000000000000000000, 1.000000000000000000 ) ) ;
#8727 = FACE_OUTER_BOUND ( 'NONE', #5738, .T. ) ;
#8728 = CONICAL_SURFACE ( 'NONE', #5256, 17.99999999999999645, 0.7853981633974447263 ) ;
#8729 = AXIS2_PLACEMENT_3D ( 'NONE', #3799, #6797, #4494 ) ;
#8730 = EDGE_CURVE ( 'NONE', #5165, #9400, #3885, .T. ) ;
#8731 = EDGE_CURVE ( 'NONE', #7747, #252, #3930, .T. ) ;
#8732 = ORIENTED_EDGE ( 'NONE', *, *, #8130, .T. ) ;
#8733 = CARTESIAN_POINT ( 'NONE',  ( -18.58791755254458167, 59.99999999999999289, -23.54759692749571087 ) ) ;
#8734 = CARTESIAN_POINT ( 'NONE',  ( 28.87459861216657231, 61.99999999999999289, 15.97678174684340924 ) ) ;
#8735 = EDGE_CURVE ( 'NONE', #9259, #7747, #8051, .T. ) ;
#8736 = ORIENTED_EDGE ( 'NONE', *, *, #5211, .T. ) ;
#8737 = DIRECTION ( 'NONE',  ( -0.000000000000000000, -0.000000000000000000, 1.000000000000000000 ) ) ;
#8738 = CARTESIAN_POINT ( 'NONE',  ( 4.531193156845207581E-15, 58.99999999999999289, 37.00000000000000711 ) ) ;
#8739 = CARTESIAN_POINT ( 'NONE',  ( 0.000000000000000000, 59.99999999999999289, 0.000000000000000000 ) ) ;
#8740 = CARTESIAN_POINT ( 'NONE',  ( 0.000000000000000000, 2.449293598294705921E-16, -1.999999999999999556 ) ) ;
#8741 = DIRECTION ( 'NONE',  ( -1.000000000000000000, 0.000000000000000000, -0.000000000000000000 ) ) ;
#8742 = ORIENTED_EDGE ( 'NONE', *, *, #4508, .F. ) ;
#8743 = FACE_BOUND ( 'NONE', #5525, .T. ) ;
#8744 = DIRECTION ( 'NONE',  ( 0.000000000000000000, 1.000000000000000000, 0.000000000000000000 ) ) ;
#8745 = ORIENTED_EDGE ( 'NONE', *, *, #2997, .T. ) ;
#8746 = CIRCLE ( 'NONE', #1804, 38.00000000000000711 ) ;
#8747 = CARTESIAN_POINT ( 'NONE',  ( 28.34870838944214100, 39.99999999999999289, 9.815840903884559765 ) ) ;
#8748 = CARTESIAN_POINT ( 'NONE',  ( -20.44670930779907891, 54.99999999999999289, -25.90235662024525709 ) ) ;
#8749 = CARTESIAN_POINT ( 'NONE',  ( 9.726904566720470768, 13.53265914481252885, 37.76886403029045169 ) ) ;
#8750 = DIRECTION ( 'NONE',  ( 1.049160758270772931E-14, 8.673617379884035472E-17, -1.000000000000000222 ) ) ;
#8751 = VECTOR ( 'NONE', #623, 1000.000000000000114 ) ;
#8752 = EDGE_LOOP ( 'NONE', ( #5101, #8791, #6273, #4299 ) ) ;
#8753 = FACE_OUTER_BOUND ( 'NONE', #1677, .T. ) ;
#8754 = ORIENTED_EDGE ( 'NONE', *, *, #6309, .F. ) ;
#8755 = DIRECTION ( 'NONE',  ( -0.000000000000000000, 1.000000000000000000, -0.000000000000000000 ) ) ;
#8756 = VERTEX_POINT ( 'NONE', #1661 ) ;
#8757 = ORIENTED_EDGE ( 'NONE', *, *, #4032, .T. ) ;
#8758 = CARTESIAN_POINT ( 'NONE',  ( -7.506866817950279547, 9.909495310584443217, 42.53598369858231365 ) ) ;
#8759 = VECTOR ( 'NONE', #5244, 1000.000000000000114 ) ;
#8760 = DIRECTION ( 'NONE',  ( -0.000000000000000000, 1.000000000000000000, -0.000000000000000000 ) ) ;
#8761 = CARTESIAN_POINT ( 'NONE',  ( 0.000000000000000000, 39.99999999999999289, 0.000000000000000000 ) ) ;
#8762 = CIRCLE ( 'NONE', #6067, 10.00000000000000000 ) ;
#8763 = VECTOR ( 'NONE', #6581, 1000.000000000000000 ) ;
#8764 = ORIENTED_EDGE ( 'NONE', *, *, #8060, .T. ) ;
#8765 = DIRECTION ( 'NONE',  ( 0.000000000000000000, 1.000000000000000000, 0.000000000000000000 ) ) ;
#8766 = VERTEX_POINT ( 'NONE', #5561 ) ;
#8767 = CIRCLE ( 'NONE', #8293, 34.50000000000000000 ) ;
#8768 = CIRCLE ( 'NONE', #4505, 26.00000000000002132 ) ;
#8769 = ORIENTED_EDGE ( 'NONE', *, *, #1792, .T. ) ;
#8770 = CARTESIAN_POINT ( 'NONE',  ( 1.300000000000000044, 1.082531754730548856, -0.6250000000000002220 ) ) ;
#8771 = FACE_OUTER_BOUND ( 'NONE', #6947, .T. ) ;
#8772 = CARTESIAN_POINT ( 'NONE',  ( 13.23285520384964009, 1.704015861027379009, 36.68641462353301108 ) ) ;
#8773 = DIRECTION ( 'NONE',  ( 0.000000000000000000, 0.000000000000000000, 1.000000000000000000 ) ) ;
#8774 = B_SPLINE_CURVE_WITH_KNOTS ( 'NONE', 3,
 ( #1448, #6479, #6821, #9750, #9060, #913, #6725, #3925, #9210, #3821, #4713, #7578, #8368, #4568 ),
 .UNSPECIFIED., .F., .F.,
 ( 4, 2, 2, 2, 2, 2, 4 ),
 ( 0.000000000000000000, 0.003068295728000690944, 0.006136591456001381888, 0.007670739320001727576, 0.009204887184002075867, 0.01073903504800242069, 0.01227318291200276898 ),
 .UNSPECIFIED. ) ;
#8775 = FACE_OUTER_BOUND ( 'NONE', #1063, .T. ) ;
#8776 = EDGE_CURVE ( 'NONE', #8583, #6663, #2132, .T. ) ;
#8777 = ADVANCED_FACE ( 'NONE', ( #1019 ), #7637, .F. ) ;
#8778 = DIRECTION ( 'NONE',  ( 0.000000000000000000, 0.000000000000000000, 1.000000000000000000 ) ) ;
#8779 =( GEOMETRIC_REPRESENTATION_CONTEXT ( 3 ) GLOBAL_UNCERTAINTY_ASSIGNED_CONTEXT ( ( #7535 ) ) GLOBAL_UNIT_ASSIGNED_CONTEXT ( ( #2749, #5770, #2695 ) ) REPRESENTATION_CONTEXT ( 'NONE', 'WORKASPACE' ) );
#8780 = ORIENTED_EDGE ( 'NONE', *, *, #2990, .T. ) ;
#8781 = DIRECTION ( 'NONE',  ( -1.820952055660014662E-28, -1.000000000000000000, -7.038118388768679669E-30 ) ) ;
#8782 = CARTESIAN_POINT ( 'NONE',  ( 8.125263811375475598, 9.132942212448577735, 42.27923313267293537 ) ) ;
#8783 = EDGE_LOOP ( 'NONE', ( #8524, #8400, #6099, #658 ) ) ;
#8784 = CYLINDRICAL_SURFACE ( 'NONE', #2087, 2.499999999999998668 ) ;
#8785 = DIRECTION ( 'NONE',  ( 0.000000000000000000, 0.000000000000000000, 1.000000000000000000 ) ) ;
#8786 = DIRECTION ( 'NONE',  ( -1.224646799147349509E-16, 0.000000000000000000, -1.000000000000000000 ) ) ;
#8787 = ADVANCED_FACE ( 'NONE', ( #830 ), #3839, .F. ) ;
#8788 = EDGE_CURVE ( 'NONE', #1527, #1789, #3231, .T. ) ;
#8789 = CARTESIAN_POINT ( 'NONE',  ( 1.148778693228098442E-26, 55.00000000000030553, -25.00000000000000000 ) ) ;
#8790 = EDGE_CURVE ( 'NONE', #8258, #8160, #5309, .T. ) ;
#8791 = ORIENTED_EDGE ( 'NONE', *, *, #2486, .T. ) ;
#8792 = PLANE ( 'NONE',  #6372 ) ;
#8793 = ORIENTED_EDGE ( 'NONE', *, *, #201, .T. ) ;
#8794 = FACE_OUTER_BOUND ( 'NONE', #8805, .T. ) ;
#8795 = ORIENTED_EDGE ( 'NONE', *, *, #235, .T. ) ;
#8796 = EDGE_CURVE ( 'NONE', #1498, #5153, #584, .T. ) ;
#8797 = CARTESIAN_POINT ( 'NONE',  ( -15.25056439471426195, 60.99999999999999289, 27.56211685706803038 ) ) ;
#8798 = CARTESIAN_POINT ( 'NONE',  ( 0.000000000000000000, 39.99999999999999289, 0.000000000000000000 ) ) ;
#8799 = EDGE_CURVE ( 'NONE', #1409, #9349, #6618, .T. ) ;
#8800 = CARTESIAN_POINT ( 'NONE',  ( 4.444319822552836641, 12.28422794470395374, 38.81412028401931025 ) ) ;
#8801 = EDGE_LOOP ( 'NONE', ( #9044, #1611, #3066, #130 ) ) ;
#8802 = CYLINDRICAL_SURFACE ( 'NONE', #7813, 4.500000000000005329 ) ;
#8803 = ORIENTED_EDGE ( 'NONE', *, *, #2623, .F. ) ;
#8804 = LINE ( 'NONE', #8203, #4974 ) ;
#8805 = EDGE_LOOP ( 'NONE', ( #2028, #7043, #6600, #8148 ) ) ;
#8806 = ORIENTED_EDGE ( 'NONE', *, *, #5874, .T. ) ;
#8807 = CARTESIAN_POINT ( 'NONE',  ( -0.8485526577698208062, 18.27243448981633023, 38.99321009875914967 ) ) ;
#8808 = CARTESIAN_POINT ( 'NONE',  ( -27.56211685706797709, 60.99999999999999289, -15.25056439471436676 ) ) ;
#8809 = CARTESIAN_POINT ( 'NONE',  ( -18.58791755254458167, 59.99999999999999289, -23.54759692749571087 ) ) ;
#8810 = ORIENTED_EDGE ( 'NONE', *, *, #8730, .F. ) ;
#8811 = CYLINDRICAL_SURFACE ( 'NONE', #7499, 40.00000000000000711 ) ;
#8812 = CARTESIAN_POINT ( 'NONE',  ( -8.545448575588382667, 54.50000000000031264, -24.55555555555560687 ) ) ;
#8813 = ORIENTED_EDGE ( 'NONE', *, *, #7087, .T. ) ;
#8814 = LINE ( 'NONE', #4184, #5818 ) ;
#8815 = EDGE_CURVE ( 'NONE', #1437, #5863, #381, .T. ) ;
#8816 = DIRECTION ( 'NONE',  ( 1.000000000000000000, -0.000000000000000000, 1.047444401652940795E-14 ) ) ;
#8817 = LINE ( 'NONE', #443, #8846 ) ;
#8818 = DIRECTION ( 'NONE',  ( -0.000000000000000000, 1.000000000000000000, -0.000000000000000000 ) ) ;
#8819 = EDGE_CURVE ( 'NONE', #1081, #6613, #4136, .T. ) ;
#8820 = CIRCLE ( 'NONE', #7070, 30.00000000000000711 ) ;
#8821 = CARTESIAN_POINT ( 'NONE',  ( 2.204364238465235033E-15, 38.99999999999993605, -17.99999999999999645 ) ) ;
#8822 = FACE_OUTER_BOUND ( 'NONE', #4075, .T. ) ;
#8823 = ORIENTED_EDGE ( 'NONE', *, *, #7831, .T. ) ;
#8824 = CARTESIAN_POINT ( 'NONE',  ( 6.000000000000007994, -15.00000000000000000, 31.00000000000000711 ) ) ;
#8825 = CARTESIAN_POINT ( 'NONE',  ( 8.957468044428361864, 7.752316930812642504, 41.89900961843087401 ) ) ;
#8826 = ORIENTED_EDGE ( 'NONE', *, *, #2723, .T. ) ;
#8827 = CYLINDRICAL_SURFACE ( 'NONE', #5234, 1.500000000000001332 ) ;
#8828 = LINE ( 'NONE', #3491, #8308 ) ;
#8829 = AXIS2_PLACEMENT_3D ( 'NONE', #9147, #6074, #4706 ) ;
#8830 = VECTOR ( 'NONE', #8816, 1000.000000000000000 ) ;
#8831 = CARTESIAN_POINT ( 'NONE',  ( -13.30503757985684565, 2.990201221717010860, 36.66029814382953589 ) ) ;
#8832 = CARTESIAN_POINT ( 'NONE',  ( 1.555535097482682654E-26, 78.08723716182652197, -25.00000000000000000 ) ) ;
#8833 = ADVANCED_FACE ( 'NONE', ( #1854, #4870 ), #612, .T. ) ;
#8834 = DIRECTION ( 'NONE',  ( -0.000000000000000000, 1.000000000000000000, -0.000000000000000000 ) ) ;
#8835 = VERTEX_POINT ( 'NONE', #5156 ) ;
#8836 = DIRECTION ( 'NONE',  ( 6.982962677686269866E-15, -0.000000000000000000, -1.000000000000000000 ) ) ;
#8837 = DIRECTION ( 'NONE',  ( -0.000000000000000000, 1.000000000000000000, -0.000000000000000000 ) ) ;
#8838 = EDGE_CURVE ( 'NONE', #279, #3425, #1047, .T. ) ;
#8839 = ORIENTED_EDGE ( 'NONE', *, *, #6791, .T. ) ;
#8840 = CIRCLE ( 'NONE', #4595, 37.00000000000000711 ) ;
#8841 = DIRECTION ( 'NONE',  ( 0.000000000000000000, 1.000000000000000000, 0.000000000000000000 ) ) ;
#8842 = EDGE_CURVE ( 'NONE', #6663, #4231, #1834, .T. ) ;
#8843 = CARTESIAN_POINT ( 'NONE',  ( -26.32489316217636954, -10.00000000000000533, 6.000000000000009770 ) ) ;
#8844 = DIRECTION ( 'NONE',  ( 1.000000000000000000, 0.000000000000000000, 0.000000000000000000 ) ) ;
#8845 = EDGE_CURVE ( 'NONE', #6406, #5750, #2913, .T. ) ;
#8846 = VECTOR ( 'NONE', #4970, 1000.000000000000000 ) ;
#8847 = ORIENTED_EDGE ( 'NONE', *, *, #8668, .T. ) ;
#8848 = DIRECTION ( 'NONE',  ( -0.000000000000000000, -1.000000000000000000, -0.000000000000000000 ) ) ;
#8849 = EDGE_CURVE ( 'NONE', #2192, #1495, #1802, .T. ) ;
#8850 = ORIENTED_EDGE ( 'NONE', *, *, #51, .T. ) ;
#8851 = DIRECTION ( 'NONE',  ( -1.820952055660014662E-28, -1.000000000000000000, -7.038118388768679669E-30 ) ) ;
#8852 = EDGE_CURVE ( 'NONE', #5208, #1486, #9640, .T. ) ;
#8853 = VERTEX_POINT ( 'NONE', #4830 ) ;
#8854 = CARTESIAN_POINT ( 'NONE',  ( -9.815840903884557989, 59.99999999999999289, 28.34870838944214455 ) ) ;
#8855 = ORIENTED_EDGE ( 'NONE', *, *, #3332, .F. ) ;
#8856 = ADVANCED_FACE ( 'NONE', ( #9596 ), #7843, .T. ) ;
#8857 = CARTESIAN_POINT ( 'NONE',  ( -8.970012219034815715, 7.764115678634449402, 41.89420632471620110 ) ) ;
#8858 = DIRECTION ( 'NONE',  ( 0.000000000000000000, 1.000000000000000000, 0.000000000000000000 ) ) ;
#8859 = AXIS2_PLACEMENT_3D ( 'NONE', #9022, #2232, #2292 ) ;
#8860 = AXIS2_PLACEMENT_3D ( 'NONE', #561, #3564, #9591 ) ;
#8861 = DIRECTION ( 'NONE',  ( 0.000000000000000000, -1.000000000000000000, 0.000000000000000000 ) ) ;
#8862 = ORIENTED_EDGE ( 'NONE', *, *, #6047, .F. ) ;
#8863 = DIRECTION ( 'NONE',  ( 0.000000000000000000, 1.000000000000000000, 0.000000000000000000 ) ) ;
#8864 = ORIENTED_EDGE ( 'NONE', *, *, #2549, .F. ) ;
#8865 = DIRECTION ( 'NONE',  ( 0.000000000000000000, 0.000000000000000000, 1.000000000000000000 ) ) ;
#8866 = CARTESIAN_POINT ( 'NONE',  ( 0.000000000000000000, 54.99999999999999289, 0.000000000000000000 ) ) ;
#8867 =( NAMED_UNIT ( * ) PLANE_ANGLE_UNIT ( ) SI_UNIT ( $, .RADIAN. ) );
#8868 = DIRECTION ( 'NONE',  ( 0.000000000000000000, -0.000000000000000000, 1.000000000000000000 ) ) ;
#8869 = AXIS2_PLACEMENT_3D ( 'NONE', #7960, #460, #9253 ) ;
#8870 = LINE ( 'NONE', #7540, #7174 ) ;
#8871 = PRODUCT_DEFINITION ( 'UNKNOWN', '', #2847, #25 ) ;
#8872 = AXIS2_PLACEMENT_3D ( 'NONE', #4745, #2495, #348 ) ;
#8873 = CARTESIAN_POINT ( 'NONE',  ( 0.000000000000000000, 59.99999999999999289, 0.000000000000000000 ) ) ;
#8874 = ORIENTED_EDGE ( 'NONE', *, *, #1487, .F. ) ;
#8875 = CARTESIAN_POINT ( 'NONE',  ( -28.87459861216645862, 60.99999999999999289, -15.97678174684361707 ) ) ;
#8876 = DIRECTION ( 'NONE',  ( 0.000000000000000000, 1.000000000000000000, 0.000000000000000000 ) ) ;
#8877 = CARTESIAN_POINT ( 'NONE',  ( 3.274489253962265867, 12.76606442083950910, 43.73447258638396562 ) ) ;
#8878 = DIRECTION ( 'NONE',  ( 0.000000000000000000, -0.7071067811865512365, -0.7071067811865439090 ) ) ;
#8879 = DIRECTION ( 'NONE',  ( -0.7071067811865573427, -0.7071067811865376918, 7.666467083416969298E-17 ) ) ;
#8880 = DIRECTION ( 'NONE',  ( 0.000000000000000000, 0.000000000000000000, -1.000000000000000000 ) ) ;
#8881 = AXIS2_PLACEMENT_3D ( 'NONE', #964, #6136, #6095 ) ;
#8882 = CONICAL_SURFACE ( 'NONE', #5252, 26.00000000000000355, 0.7853981633974346233 ) ;
#8883 = CARTESIAN_POINT ( 'NONE',  ( -8.545448575588412865, -1.753174028375700797E-27, -24.55555555555569569 ) ) ;
#8884 = CARTESIAN_POINT ( 'NONE',  ( 9.318419442923201951E-27, 44.00000000000019895, -25.00000000000000000 ) ) ;
#8885 = DIRECTION ( 'NONE',  ( -0.000000000000000000, -1.000000000000000000, -0.000000000000000000 ) ) ;
#8886 = ORIENTED_EDGE ( 'NONE', *, *, #6780, .T. ) ;
#8887 = CARTESIAN_POINT ( 'NONE',  ( -2.094888803305880518E-13, 39.99999999999999289, 30.00000000000000711 ) ) ;
#8888 = CARTESIAN_POINT ( 'NONE',  ( -0.9067368948456047129, -14.99999999999999822, 30.49541815531657818 ) ) ;
#8889 = EDGE_CURVE ( 'NONE', #9543, #2719, #2867, .T. ) ;
#8890 = VERTEX_POINT ( 'NONE', #7422 ) ;
#8891 = DIRECTION ( 'NONE',  ( -0.000000000000000000, -1.000000000000000000, -0.000000000000000000 ) ) ;
#8892 = DIRECTION ( 'NONE',  ( 0.9588120495101036811, 9.854661834794498374E-17, 0.2840412887490736393 ) ) ;
#8893 = EDGE_LOOP ( 'NONE', ( #6181, #1624, #9260, #5280 ) ) ;
#8894 = CARTESIAN_POINT ( 'NONE',  ( 5.316540241612734974, 11.77069107846751095, 43.27322217794340986 ) ) ;
#8895 = PRODUCT_CONTEXT ( 'NONE', #1076, 'mechanical' ) ;
#8896 = ORIENTED_EDGE ( 'NONE', *, *, #1288, .F. ) ;
#8897 = CARTESIAN_POINT ( 'NONE',  ( -8.545448575588372009, -1.756640702275597822E-27, -24.55555555555557845 ) ) ;
#8898 = ORIENTED_EDGE ( 'NONE', *, *, #2231, .T. ) ;
#8899 = DIRECTION ( 'NONE',  ( -0.000000000000000000, -1.000000000000000000, -0.000000000000000000 ) ) ;
#8900 = EDGE_LOOP ( 'NONE', ( #8494, #6170, #1870, #466 ) ) ;
#8901 = DIRECTION ( 'NONE',  ( 0.000000000000000000, -1.000000000000000000, -0.000000000000000000 ) ) ;
#8902 = AXIS2_PLACEMENT_3D ( 'NONE', #5182, #2348, #4444 ) ;
#8903 = EDGE_LOOP ( 'NONE', ( #2893, #1308, #5277, #8337 ) ) ;
#8904 = CARTESIAN_POINT ( 'NONE',  ( -4.284152118168920609, 17.52839865830862820, 38.77238817881250554 ) ) ;
#8905 = CARTESIAN_POINT ( 'NONE',  ( 4.000000000000001776, 30.00000000000000000, -24.67792535850613334 ) ) ;
#8906 = DIRECTION ( 'NONE',  ( -0.3286710990610922090, -6.289316826390952918E-29, -0.9444444444444435316 ) ) ;
#8907 = ADVANCED_FACE ( 'NONE', ( #7885 ), #5662, .F. ) ;
#8908 = EDGE_CURVE ( 'NONE', #6352, #5845, #4314, .T. ) ;
#8909 = VECTOR ( 'NONE', #6717, 1000.000000000000114 ) ;
#8910 = EDGE_CURVE ( 'NONE', #7071, #3135, #8064, .T. ) ;
#8911 = AXIS2_PLACEMENT_3D ( 'NONE', #4208, #8834, #4992 ) ;
#8912 = ADVANCED_FACE ( 'NONE', ( #1346 ), #8674, .F. ) ;
#8913 = ORIENTED_EDGE ( 'NONE', *, *, #4642, .T. ) ;
#8914 = CARTESIAN_POINT ( 'NONE',  ( -6.000000000000005329, -10.00000000000000533, -26.32489316217636954 ) ) ;
#8915 = EDGE_LOOP ( 'NONE', ( #739, #6517, #69, #5409, #3304, #8295, #2578, #7762, #238, #5381, #6777, #8027, #7219, #619, #2730, #1332 ) ) ;
#8916 = CIRCLE ( 'NONE', #9548, 1.500000000000001332 ) ;
#8917 = DIRECTION ( 'NONE',  ( -1.000000000000000000, 0.000000000000000000, -0.000000000000000000 ) ) ;
#8918 = CIRCLE ( 'NONE', #4348, 19.00000000000000355 ) ;
#8919 = DIRECTION ( 'NONE',  ( 0.000000000000000000, 0.000000000000000000, 1.000000000000000000 ) ) ;
#8920 = LINE ( 'NONE', #5851, #4666 ) ;
#8921 = VECTOR ( 'NONE', #1291, 1000.000000000000000 ) ;
#8922 = AXIS2_PLACEMENT_3D ( 'NONE', #4955, #471, #6469 ) ;
#8923 = CIRCLE ( 'NONE', #5912, 30.00000000000000711 ) ;
#8924 = VECTOR ( 'NONE', #475, 1000.000000000000000 ) ;
#8925 = LINE ( 'NONE', #6678, #2356 ) ;
#8926 = ORIENTED_EDGE ( 'NONE', *, *, #6896, .T. ) ;
#8927 = CARTESIAN_POINT ( 'NONE',  ( -8.106025752690484865, 61.92736406916336733, 36.79170325027453714 ) ) ;
#8928 = CARTESIAN_POINT ( 'NONE',  ( 0.000000000000000000, 59.99999999999999289, 0.000000000000000000 ) ) ;
#8929 = DIRECTION ( 'NONE',  ( 0.000000000000000000, 0.000000000000000000, -1.000000000000000000 ) ) ;
#8930 = AXIS2_PLACEMENT_3D ( 'NONE', #6946, #208, #7511 ) ;
#8931 = CARTESIAN_POINT ( 'NONE',  ( -1.783505000977663846, -14.99999999999999822, 30.27207879089416664 ) ) ;
#8932 = CARTESIAN_POINT ( 'NONE',  ( -8.216777476527294510, 55.00000000000030553, -23.61111111111111427 ) ) ;
#8933 = VECTOR ( 'NONE', #7153, 1000.000000000000000 ) ;
#8934 = DIRECTION ( 'NONE',  ( 0.000000000000000000, -1.000000000000000000, 0.000000000000000000 ) ) ;
#8935 = VECTOR ( 'NONE', #3205, 1000.000000000000000 ) ;
#8936 = CARTESIAN_POINT ( 'NONE',  ( 31.00000000000000711, 27.80235549540589801, 4.012532818320192263 ) ) ;
#8937 = EDGE_LOOP ( 'NONE', ( #9570, #1958, #5611, #6401 ) ) ;
#8938 = DIRECTION ( 'NONE',  ( 0.000000000000000000, 0.000000000000000000, 1.000000000000000000 ) ) ;
#8939 = ADVANCED_FACE ( 'NONE', ( #4371, #7374 ), #1299, .T. ) ;
#8940 = ORIENTED_EDGE ( 'NONE', *, *, #890, .T. ) ;
#8941 = CARTESIAN_POINT ( 'NONE',  ( 6.439978105601112524E-15, 18.29485247664131009, 39.00000000000002132 ) ) ;
#8942 = CARTESIAN_POINT ( 'NONE',  ( 8.639162863793341529, -6.583298275952675915, 38.16418810910280968 ) ) ;
#8943 = EDGE_LOOP ( 'NONE', ( #424, #1684 ) ) ;
#8944 = B_SPLINE_CURVE_WITH_KNOTS ( 'NONE', 3,
 ( #5651, #1054, #1744, #4073, #7771, #7063, #1006, #7420, #1438, #5100, #2717, #2815, #1984, #704, #6661, #9686, #5006, #657, #7314, #6616, #6573, #3714, #7469, #3663, #5929, #2911, #1251, #8107, #565, #8952, #9492, #9638 ),
 .UNSPECIFIED., .F., .F.,
 ( 4, 2, 2, 2, 2, 2, 2, 2, 2, 2, 2, 2, 2, 2, 2, 4 ),
 ( 0.001042552523569530588, 0.002052900844284174554, 0.002558075004641499357, 0.003063249164998824593, 0.003568423325356149395, 0.004073597485713474631, 0.004578771646070799867, 0.005083945806428125103, 0.005589119966785450339, 0.006094294127142775575, 0.006599468287500100810, 0.007104642447857426046, 0.007609816608214751282, 0.008114990768572076518, 0.008620164928929401754, 0.009125339089286726990 ),
 .UNSPECIFIED. ) ;
#8945 = DIRECTION ( 'NONE',  ( -1.820952055660014662E-28, -1.000000000000000000, -7.038118388768679669E-30 ) ) ;
#8946 = DIRECTION ( 'NONE',  ( 1.000000000000000000, 0.000000000000000000, 1.079383496163345602E-14 ) ) ;
#8947 = VERTEX_POINT ( 'NONE', #3762 ) ;
#8948 = CARTESIAN_POINT ( 'NONE',  ( 8.149741407064750476, -2.543282342078551306, 38.27864742387711772 ) ) ;
#8949 = ORIENTED_EDGE ( 'NONE', *, *, #5284, .F. ) ;
#8950 = CARTESIAN_POINT ( 'NONE',  ( 33.06426808735054124, 60.99999999999999289, 5.562309845534586294 ) ) ;
#8951 = ORIENTED_EDGE ( 'NONE', *, *, #8430, .T. ) ;
#8952 = CARTESIAN_POINT ( 'NONE',  ( 33.40276010569236576, 59.97308474266854716, 3.079737114311560386 ) ) ;
#8953 = VERTEX_POINT ( 'NONE', #6077 ) ;
#8954 = CARTESIAN_POINT ( 'NONE',  ( 9.815840903884561541, 39.99999999999999289, -28.34870838944214100 ) ) ;
#8955 = EDGE_LOOP ( 'NONE', ( #3376, #9041, #914, #3292, #2631 ) ) ;
#8956 = CARTESIAN_POINT ( 'NONE',  ( -8.659653037499971617, 8.337804354671460416, 42.04276546470546805 ) ) ;
#8957 = DIRECTION ( 'NONE',  ( -1.000000000000000000, -0.000000000000000000, -0.000000000000000000 ) ) ;
#8958 = CARTESIAN_POINT ( 'NONE',  ( -8.216777476527294510, 52.00000000000031974, -23.61111111111111427 ) ) ;
#8959 = EDGE_CURVE ( 'NONE', #909, #2914, #7523, .T. ) ;
#8960 = VERTEX_POINT ( 'NONE', #2365 ) ;
#8961 = DIRECTION ( 'NONE',  ( -0.000000000000000000, 1.000000000000000000, -0.000000000000000000 ) ) ;
#8962 = DIRECTION ( 'NONE',  ( 0.000000000000000000, 0.000000000000000000, 1.000000000000000000 ) ) ;
#8963 = EDGE_LOOP ( 'NONE', ( #2559, #7942, #9451, #8111 ) ) ;
#8964 = EDGE_CURVE ( 'NONE', #9341, #577, #9097, .T. ) ;
#8965 = CARTESIAN_POINT ( 'NONE',  ( 0.000000000000000000, 28.99999999999997158, 0.000000000000000000 ) ) ;
#8966 = DIRECTION ( 'NONE',  ( 0.000000000000000000, 1.000000000000000000, 0.000000000000000000 ) ) ;
#8967 = ADVANCED_FACE ( 'NONE', ( #168 ), #5398, .T. ) ;
#8968 = PRESENTATION_STYLE_ASSIGNMENT (( #2935 ) ) ;
#8969 = ADVANCED_FACE ( 'NONE', ( #5931 ), #6813, .F. ) ;
#8970 = CARTESIAN_POINT ( 'NONE',  ( 2.200000000000000622, 2.694222958124176513E-16, -2.199999999999999734 ) ) ;
#8971 = EDGE_LOOP ( 'NONE', ( #7119, #236, #2801, #9269, #5740, #310 ) ) ;
#8972 = DIRECTION ( 'NONE',  ( 0.9860132971832693549, 1.788557213313974126E-28, -0.1666666666666657970 ) ) ;
#8973 = CARTESIAN_POINT ( 'NONE',  ( 5.030598735306972102, -5.371835421513210029, 43.35589067224919546 ) ) ;
#8974 = LINE ( 'NONE', #5902, #1023 ) ;
#8975 = EDGE_CURVE ( 'NONE', #5960, #9622, #3716, .T. ) ;
#8976 = PLANE ( 'NONE',  #6169 ) ;
#8977 = CARTESIAN_POINT ( 'NONE',  ( 31.00000000000000711, 27.42469319230600533, -6.000000000000006217 ) ) ;
#8978 = ADVANCED_FACE ( 'NONE', ( #1485 ), #2164, .T. ) ;
#8979 = LINE ( 'NONE', #8284, #9231 ) ;
#8980 = DIRECTION ( 'NONE',  ( -0.1666666666666658525, -3.897465909857536228E-29, -0.9860132971832695770 ) ) ;
#8981 = VECTOR ( 'NONE', #1755, 1000.000000000000000 ) ;
#8982 = CARTESIAN_POINT ( 'NONE',  ( 0.000000000000000000, 59.99999999999999289, 0.000000000000000000 ) ) ;
#8983 = ORIENTED_EDGE ( 'NONE', *, *, #2617, .T. ) ;
#8984 = CARTESIAN_POINT ( 'NONE',  ( 5.562309845534588959, 49.99999999999999289, -30.56426808735054479 ) ) ;
#8985 = CARTESIAN_POINT ( 'NONE',  ( 11.07761026121385939, -5.000000000000008882, 37.39366993089406321 ) ) ;
#8986 = VERTEX_POINT ( 'NONE', #7570 ) ;
#8987 = CARTESIAN_POINT ( 'NONE',  ( -8.216777476527294510, 41.50000000000020606, -23.61111111111111427 ) ) ;
#8988 = AXIS2_PLACEMENT_3D ( 'NONE', #7730, #239, #2226 ) ;
#8989 = DIRECTION ( 'NONE',  ( 0.2840412887490735838, 0.000000000000000000, -0.9588120495101035701 ) ) ;
#8990 = ORIENTED_EDGE ( 'NONE', *, *, #8512, .T. ) ;
#8991 = EDGE_CURVE ( 'NONE', #5845, #4065, #3726, .T. ) ;
#8992 = CARTESIAN_POINT ( 'NONE',  ( 9.079125748275108876, -7.673965757712833735, 37.92978250830171305 ) ) ;
#8993 = APPLICATION_PROTOCOL_DEFINITION ( 'draft international standard', 'automotive_design', 1998, #6802 ) ;
#8994 = VERTEX_POINT ( 'NONE', #8954 ) ;
#8995 = ORIENTED_EDGE ( 'NONE', *, *, #7081, .F. ) ;
#8996 = DIRECTION ( 'NONE',  ( 0.9860132971832693549, 1.788557213313974126E-28, -0.1666666666666657970 ) ) ;
#8997 = ORIENTED_EDGE ( 'NONE', *, *, #3312, .T. ) ;
#8998 = DIRECTION ( 'NONE',  ( -1.820952055660014662E-28, -1.000000000000000000, -7.038118388768679669E-30 ) ) ;
#8999 = VERTEX_POINT ( 'NONE', #6124 ) ;
#9000 = FACE_OUTER_BOUND ( 'NONE', #9020, .T. ) ;
#9001 = AXIS2_PLACEMENT_3D ( 'NONE', #2976, #5850, #6629 ) ;
#9002 = ORIENTED_EDGE ( 'NONE', *, *, #8544, .T. ) ;
#9003 = CARTESIAN_POINT ( 'NONE',  ( -6.605258697374647880, 10.83052367162449769, 42.87576923823134223 ) ) ;
#9004 = CARTESIAN_POINT ( 'NONE',  ( 33.06426808735054124, 59.99999999999999289, 5.562309845534586294 ) ) ;
#9005 = CARTESIAN_POINT ( 'NONE',  ( 9.811457508686334330E-27, 54.50000000000031264, -26.00000000000004974 ) ) ;
#9006 = B_SPLINE_CURVE_WITH_KNOTS ( 'NONE', 3,
 ( #1505, #1232, #5988, #4248, #6034, #2283, #7950, #7248, #497, #6504, #9526, #2751, #7484, #550 ),
 .UNSPECIFIED., .F., .F.,
 ( 4, 2, 2, 2, 2, 2, 4 ),
 ( 0.01227318291200276898, 0.01534032230130411359, 0.01687389199595478589, 0.01840746169060545820, 0.02147460107990680628, 0.02300817077455747511, 0.02454174046920814395 ),
 .UNSPECIFIED. ) ;
#9007 = AXIS2_PLACEMENT_3D ( 'NONE', #8705, #2810, #9539 ) ;
#9008 = ORIENTED_EDGE ( 'NONE', *, *, #825, .F. ) ;
#9009 = CARTESIAN_POINT ( 'NONE',  ( -7.766845228004613411, 59.52671121465667881, 34.26018231648108525 ) ) ;
#9010 = UNCERTAINTY_MEASURE_WITH_UNIT (LENGTH_MEASURE( 1.000000000000000082E-05 ), #6981, 'distance_accuracy_value', 'NONE');
#9011 = VERTEX_POINT ( 'NONE', #8312 ) ;
#9012 = CARTESIAN_POINT ( 'NONE',  ( 5.137569555611264605, 60.99999999999999289, 32.59762842694627949 ) ) ;
#9013 = PLANE ( 'NONE',  #2684 ) ;
#9014 = EDGE_CURVE ( 'NONE', #6613, #2714, #3864, .T. ) ;
#9015 = DIRECTION ( 'NONE',  ( -0.000000000000000000, 1.000000000000000000, -0.000000000000000000 ) ) ;
#9016 = LINE ( 'NONE', #1182, #3826 ) ;
#9017 = ADVANCED_FACE ( 'NONE', ( #3919 ), #5348, .F. ) ;
#9018 = EDGE_CURVE ( 'NONE', #1478, #4857, #8257, .T. ) ;
#9019 = CARTESIAN_POINT ( 'NONE',  ( -4.007921376381017531, 27.80323177039520388, 31.00000000000000711 ) ) ;
#9020 = EDGE_LOOP ( 'NONE', ( #9117, #4465 ) ) ;
#9021 = CARTESIAN_POINT ( 'NONE',  ( 2.400000000000000799, 0.000000000000000000, 0.000000000000000000 ) ) ;
#9022 = CARTESIAN_POINT ( 'NONE',  ( 0.000000000000000000, 58.99999999999999289, -37.00000000000000711 ) ) ;
#9023 = CIRCLE ( 'NONE', #5861, 4.500000000000004441 ) ;
#9024 = CARTESIAN_POINT ( 'NONE',  ( -8.216777476527274970, 78.08723716182652197, -23.61111111111111427 ) ) ;
#9025 = CONICAL_SURFACE ( 'NONE', #5709, 1.610000000000000098, 0.7853981633974463916 ) ;
#9026 = CARTESIAN_POINT ( 'NONE',  ( 0.1742879017051222057, -14.99999999999999822, 30.58239647876216338 ) ) ;
#9027 = PLANE ( 'NONE',  #8530 ) ;
#9028 = ORIENTED_EDGE ( 'NONE', *, *, #8541, .F. ) ;
#9029 = CARTESIAN_POINT ( 'NONE',  ( -3.203813853954870616, 17.85736785735978671, 38.86945905611829488 ) ) ;
#9030 = CIRCLE ( 'NONE', #1303, 39.00000000000002132 ) ;
#9031 = EDGE_CURVE ( 'NONE', #6521, #667, #8356, .T. ) ;
#9032 = EDGE_CURVE ( 'NONE', #4372, #9299, #129, .T. ) ;
#9033 = EDGE_CURVE ( 'NONE', #9475, #1842, #5475, .T. ) ;
#9034 = ORIENTED_EDGE ( 'NONE', *, *, #9573, .F. ) ;
#9035 = CARTESIAN_POINT ( 'NONE',  ( 3.429011037612588487E-15, 59.99999999999999289, 27.99999999999999289 ) ) ;
#9036 = ORIENTED_EDGE ( 'NONE', *, *, #5991, .T. ) ;
#9037 = DIRECTION ( 'NONE',  ( 1.000000000000000000, 0.000000000000000000, 0.000000000000000000 ) ) ;
#9038 = CARTESIAN_POINT ( 'NONE',  ( 10.23892364353549134, -5.543295408803479596, 37.65277200319494000 ) ) ;
#9039 = AXIS2_PLACEMENT_3D ( 'NONE', #8374, #7727, #6828 ) ;
#9040 = VECTOR ( 'NONE', #5085, 1000.000000000000000 ) ;
#9041 = ORIENTED_EDGE ( 'NONE', *, *, #2240, .F. ) ;
#9042 = DIRECTION ( 'NONE',  ( 0.9860132971832693549, 1.788557213313974126E-28, -0.1666666666666657970 ) ) ;
#9043 = DIRECTION ( 'NONE',  ( 1.735493991486225692E-29, 0.000000000000000000, -1.000000000000000000 ) ) ;
#9044 = ORIENTED_EDGE ( 'NONE', *, *, #950, .T. ) ;
#9045 = CARTESIAN_POINT ( 'NONE',  ( 11.93007620353410658, 9.934074206894875303, 37.13110854819542794 ) ) ;
#9046 =( NAMED_UNIT ( * ) PLANE_ANGLE_UNIT ( ) SI_UNIT ( $, .RADIAN. ) );
#9047 = ORIENTED_EDGE ( 'NONE', *, *, #9018, .T. ) ;
#9048 = ORIENTED_EDGE ( 'NONE', *, *, #5413, .F. ) ;
#9049 = DIRECTION ( 'NONE',  ( -0.000000000000000000, -1.000000000000000000, -0.000000000000000000 ) ) ;
#9050 = CARTESIAN_POINT ( 'NONE',  ( -25.51470164434615029, 30.00000000000000000, 5.000000000000010658 ) ) ;
#9051 = CARTESIAN_POINT ( 'NONE',  ( -9.815840903884557989, 39.99999999999999289, 28.34870838944214455 ) ) ;
#9052 = ORIENTED_EDGE ( 'NONE', *, *, #8185, .F. ) ;
#9053 = DIRECTION ( 'NONE',  ( -1.820952055660014662E-28, -1.000000000000000000, -7.038118388768679669E-30 ) ) ;
#9054 = EDGE_LOOP ( 'NONE', ( #6304, #8045, #8497, #6831, #958 ) ) ;
#9055 = DIRECTION ( 'NONE',  ( 8.659560562354904508E-17, -0.7071067811865500152, 0.7071067811865451302 ) ) ;
#9056 = CARTESIAN_POINT ( 'NONE',  ( -6.000000000000005329, 30.00000000000000000, -28.37252191822215863 ) ) ;
#9057 = CARTESIAN_POINT ( 'NONE',  ( -10.00000000000001599, 3.294852476658805873, 41.36423575989289247 ) ) ;
#9058 = AXIS2_PLACEMENT_3D ( 'NONE', #7556, #7500, #5956 ) ;
#9059 = VERTEX_POINT ( 'NONE', #908 ) ;
#9060 = CARTESIAN_POINT ( 'NONE',  ( -6.878531448062598308, -7.640523322561358910, 38.67977308254881308 ) ) ;
#9061 = DIRECTION ( 'NONE',  ( -1.084202172485503448E-16, 0.000000000000000000, -1.000000000000000000 ) ) ;
#9062 = ORIENTED_EDGE ( 'NONE', *, *, #3474, .T. ) ;
#9063 = ORIENTED_EDGE ( 'NONE', *, *, #7270, .T. ) ;
#9064 = CIRCLE ( 'NONE', #3691, 31.49999999999999289 ) ;
#9065 = DIRECTION ( 'NONE',  ( -6.982962677686274599E-15, 0.000000000000000000, 1.000000000000000000 ) ) ;
#9066 = LINE ( 'NONE', #5260, #5274 ) ;
#9067 = VECTOR ( 'NONE', #7599, 1000.000000000000000 ) ;
#9068 = CIRCLE ( 'NONE', #8117, 31.50000000000000000 ) ;
#9069 = DIRECTION ( 'NONE',  ( -1.735493991486225972E-29, 6.508102468073347395E-30, 1.000000000000000000 ) ) ;
#9070 = PRODUCT_DEFINITION_SHAPE ( 'NONE', 'NONE',  #9756 ) ;
#9071 = EDGE_LOOP ( 'NONE', ( #5089, #8648, #6650, #9 ) ) ;
#9072 = CARTESIAN_POINT ( 'NONE',  ( -30.00000000000000711, 30.00000000000000000, -4.999999999999997335 ) ) ;
#9073 = VECTOR ( 'NONE', #4267, 1000.000000000000000 ) ;
#9074 = AXIS2_PLACEMENT_3D ( 'NONE', #4594, #1757, #3090 ) ;
#9075 = VERTEX_POINT ( 'NONE', #755 ) ;
#9076 = DIRECTION ( 'NONE',  ( -1.000000000000000000, 0.000000000000000000, -0.000000000000000000 ) ) ;
#9077 = CARTESIAN_POINT ( 'NONE',  ( -8.545448575588377338, 49.00000000000032685, -24.55555555555561043 ) ) ;
#9078 = CARTESIAN_POINT ( 'NONE',  ( 7.536700119255284491, -15.00000000000000000, 28.01306679336680006 ) ) ;
#9079 = DIRECTION ( 'NONE',  ( -1.000000000000000000, -0.000000000000000000, -0.000000000000000000 ) ) ;
#9080 = FACE_OUTER_BOUND ( 'NONE', #1392, .T. ) ;
#9081 = EDGE_LOOP ( 'NONE', ( #189, #8757, #1643, #846 ) ) ;
#9082 = DIRECTION ( 'NONE',  ( -0.000000000000000000, 1.000000000000000000, -0.000000000000000000 ) ) ;
#9083 = AXIS2_PLACEMENT_3D ( 'NONE', #7115, #4906, #9402 ) ;
#9084 = AXIS2_PLACEMENT_3D ( 'NONE', #3467, #1932, #368 ) ;
#9085 = CIRCLE ( 'NONE', #5761, 39.00000000000002132 ) ;
#9086 = DIRECTION ( 'NONE',  ( 1.820952055660014662E-28, 1.000000000000000000, -6.508102468073347395E-30 ) ) ;
#9087 = AXIS2_PLACEMENT_3D ( 'NONE', #5635, #4005, #212 ) ;
#9088 = DIRECTION ( 'NONE',  ( 0.000000000000000000, 0.000000000000000000, -1.000000000000000000 ) ) ;
#9089 = EDGE_LOOP ( 'NONE', ( #9637, #6633, #8101, #1086, #8263 ) ) ;
#9090 = LINE ( 'NONE', #3293, #4942 ) ;
#9091 = CARTESIAN_POINT ( 'NONE',  ( 7.618647048773172337, -7.203156711660245293, 38.46734435507664074 ) ) ;
#9092 = VERTEX_POINT ( 'NONE', #5199 ) ;
#9093 = EDGE_CURVE ( 'NONE', #1276, #6362, #8205, .T. ) ;
#9094 = ADVANCED_FACE ( 'NONE', ( #9000 ), #2209, .T. ) ;
#9095 = EDGE_CURVE ( 'NONE', #3425, #279, #736, .T. ) ;
#9096 = DIRECTION ( 'NONE',  ( 0.000000000000000000, 0.000000000000000000, 1.000000000000000000 ) ) ;
#9097 = CIRCLE ( 'NONE', #4206, 10.00000000000001599 ) ;
#9098 = DIRECTION ( 'NONE',  ( 0.000000000000000000, 1.000000000000000000, 0.000000000000000000 ) ) ;
#9099 = VERTEX_POINT ( 'NONE', #7759 ) ;
#9100 = CARTESIAN_POINT ( 'NONE',  ( 9.655005590677982141, 0.6701487737192702854, 41.54853162078376982 ) ) ;
#9101 = ORIENTED_EDGE ( 'NONE', *, *, #8849, .F. ) ;
#9102 = EDGE_LOOP ( 'NONE', ( #2811, #6018, #858, #5367 ) ) ;
#9103 = LINE ( 'NONE', #6015, #4207 ) ;
#9104 = AXIS2_PLACEMENT_3D ( 'NONE', #4661, #7670, #4512 ) ;
#9105 = CYLINDRICAL_SURFACE ( 'NONE', #3780, 25.00000000000000000 ) ;
#9106 = CARTESIAN_POINT ( 'NONE',  ( 6.000000000000007994, 29.14236109046821710, 29.24912810952613640 ) ) ;
#9107 = ORIENTED_EDGE ( 'NONE', *, *, #868, .F. ) ;
#9108 = DIRECTION ( 'NONE',  ( 0.000000000000000000, 1.000000000000000000, 0.000000000000000000 ) ) ;
#9109 = ORIENTED_EDGE ( 'NONE', *, *, #8287, .F. ) ;
#9110 = EDGE_CURVE ( 'NONE', #3204, #3167, #6094, .T. ) ;
#9111 = DIRECTION ( 'NONE',  ( -1.820952055660014662E-28, -1.000000000000000000, -7.038118388768679669E-30 ) ) ;
#9112 = ADVANCED_FACE ( 'NONE', ( #7809 ), #268, .F. ) ;
#9113 = LINE ( 'NONE', #1490, #7020 ) ;
#9114 = CARTESIAN_POINT ( 'NONE',  ( -8.670365033978340463, -1.729970272750784410, 42.03780558699289571 ) ) ;
#9115 = VERTEX_POINT ( 'NONE', #2505 ) ;
#9116 = DIRECTION ( 'NONE',  ( -0.000000000000000000, 0.5000000000000002220, -0.8660254037844384856 ) ) ;
#9117 = ORIENTED_EDGE ( 'NONE', *, *, #3146, .T. ) ;
#9118 = VERTEX_POINT ( 'NONE', #8650 ) ;
#9119 = CARTESIAN_POINT ( 'NONE',  ( -2.303357589342566847, -6.441777582968667204, 43.86679826992887143 ) ) ;
#9120 = DIRECTION ( 'NONE',  ( 0.000000000000000000, 0.000000000000000000, -1.000000000000000000 ) ) ;
#9121 = B_SPLINE_CURVE_WITH_KNOTS ( 'NONE', 3,
 ( #1258, #7976, #4273, #7271 ),
 .UNSPECIFIED., .F., .F.,
 ( 4, 4 ),
 ( 0.000000000000000000, 0.003679109433542032855 ),
 .UNSPECIFIED. ) ;
#9122 = EDGE_CURVE ( 'NONE', #4514, #5836, #1872, .T. ) ;
#9123 = ORIENTED_EDGE ( 'NONE', *, *, #952, .F. ) ;
#9124 = CARTESIAN_POINT ( 'NONE',  ( 24.67792535850613334, 28.99999999999997158, -4.000000000000006217 ) ) ;
#9125 = CARTESIAN_POINT ( 'NONE',  ( -3.999999999999999112, 30.00000000000000000, 24.67792535850613334 ) ) ;
#9126 = VERTEX_POINT ( 'NONE', #309 ) ;
#9127 = CARTESIAN_POINT ( 'NONE',  ( 0.000000000000000000, -1.443375672974064328, -9.326206579303807412E-18 ) ) ;
#9128 = CARTESIAN_POINT ( 'NONE',  ( 5.562309845551833831, 59.00253480853272947, -35.56426808735054834 ) ) ;
#9129 = CARTESIAN_POINT ( 'NONE',  ( 33.06426808735054124, 60.99999999999999289, 5.562309845534586294 ) ) ;
#9130 = CARTESIAN_POINT ( 'NONE',  ( 0.02451486836956002016, 18.29482697815588566, 38.99999229514322252 ) ) ;
#9131 = CYLINDRICAL_SURFACE ( 'NONE', #5987, 26.00000000000012790 ) ;
#9132 = ORIENTED_EDGE ( 'NONE', *, *, #9566, .F. ) ;
#9133 = CARTESIAN_POINT ( 'NONE',  ( 26.32489316217636954, -10.00000000000000711, 6.000000000000000000 ) ) ;
#9134 = DIRECTION ( 'NONE',  ( 0.000000000000000000, -1.000000000000000000, -0.000000000000000000 ) ) ;
#9135 = DIRECTION ( 'NONE',  ( 0.6195972517514869438, -1.387778780781445281E-15, 0.7849198975831893632 ) ) ;
#9136 = EDGE_LOOP ( 'NONE', ( #9008, #1141, #3358, #9209, #3713, #898, #2959, #9201, #202, #5749, #3053, #2676 ) ) ;
#9137 = PLANE ( 'NONE',  #6503 ) ;
#9138 = CARTESIAN_POINT ( 'NONE',  ( 2.084579453908214308, -15.00000000000063061, 36.76935723448232096 ) ) ;
#9139 = ORIENTED_EDGE ( 'NONE', *, *, #6961, .F. ) ;
#9140 = EDGE_CURVE ( 'NONE', #3264, #4918, #357, .T. ) ;
#9141 = DIRECTION ( 'NONE',  ( 1.820952055660014662E-28, 1.000000000000000000, -6.508102468073347395E-30 ) ) ;
#9142 = FACE_OUTER_BOUND ( 'NONE', #8168, .T. ) ;
#9143 = CARTESIAN_POINT ( 'NONE',  ( 7.930104434999360130, -2.832236619497283669, 42.36545191093337337 ) ) ;
#9144 = ORIENTED_EDGE ( 'NONE', *, *, #2670, .T. ) ;
#9145 = DIRECTION ( 'NONE',  ( 0.000000000000000000, 0.000000000000000000, -1.000000000000000000 ) ) ;
#9146 = EDGE_CURVE ( 'NONE', #4753, #9229, #6711, .T. ) ;
#9147 = CARTESIAN_POINT ( 'NONE',  ( -5.137569555611031014, 61.99999999999999289, -32.59762842694632212 ) ) ;
#9148 = CARTESIAN_POINT ( 'NONE',  ( 24.67792535850613334, 28.99999999999997158, 4.000000000000000888 ) ) ;
#9149 = ORIENTED_EDGE ( 'NONE', *, *, #3870, .F. ) ;
#9150 = CARTESIAN_POINT ( 'NONE',  ( -2.666666666666695384, 27.66666666666662522, -27.66666666666669272 ) ) ;
#9151 = ORIENTED_EDGE ( 'NONE', *, *, #2646, .F. ) ;
#9152 = CARTESIAN_POINT ( 'NONE',  ( -5.008074634385680568, 27.61318074145110302, -31.00000000000001066 ) ) ;
#9153 = VECTOR ( 'NONE', #876, 1000.000000000000227 ) ;
#9154 = VECTOR ( 'NONE', #5847, 1000.000000000000000 ) ;
#9155 = VECTOR ( 'NONE', #3737, 1000.000000000000000 ) ;
#9156 = DIRECTION ( 'NONE',  ( 0.000000000000000000, 0.000000000000000000, -1.000000000000000000 ) ) ;
#9157 = CYLINDRICAL_SURFACE ( 'NONE', #1318, 34.50000000000000000 ) ;
#9158 = EDGE_CURVE ( 'NONE', #5111, #7767, #4851, .T. ) ;
#9159 = EDGE_CURVE ( 'NONE', #1536, #1139, #6565, .T. ) ;
#9160 = APPLICATION_CONTEXT ( 'automotive_design' ) ;
#9161 = VECTOR ( 'NONE', #4682, 1000.000000000000000 ) ;
#9162 = ORIENTED_EDGE ( 'NONE', *, *, #4393, .F. ) ;
#9163 = CARTESIAN_POINT ( 'NONE',  ( -7.420105108763661583, 59.31303094616893645, 34.74949143486232828 ) ) ;
#9164 = ORIENTED_EDGE ( 'NONE', *, *, #7831, .F. ) ;
#9165 = ORIENTED_EDGE ( 'NONE', *, *, #8908, .T. ) ;
#9166 = CARTESIAN_POINT ( 'NONE',  ( -0.01963426291157483600, -6.705128248126140278, 43.99999014335539016 ) ) ;
#9167 = PLANE ( 'NONE',  #6389 ) ;
#9168 = CIRCLE ( 'NONE', #644, 5.000000000000000888 ) ;
#9169 = CARTESIAN_POINT ( 'NONE',  ( -5.562309845551829390, 59.00253480853272947, 35.56426808735054834 ) ) ;
#9170 = VERTEX_POINT ( 'NONE', #5541 ) ;
#9171 = FACE_OUTER_BOUND ( 'NONE', #6750, .T. ) ;
#9172 = CARTESIAN_POINT ( 'NONE',  ( -9.815840903884557989, 59.99999999999999289, 28.34870838944214455 ) ) ;
#9173 = AXIS2_PLACEMENT_3D ( 'NONE', #1309, #7477, #1400 ) ;
#9174 = CIRCLE ( 'NONE', #5066, 37.99999999999999289 ) ;
#9175 = VERTEX_POINT ( 'NONE', #3360 ) ;
#9176 = CARTESIAN_POINT ( 'NONE',  ( -8.545448575588382667, -1.755677737303404204E-27, -24.55555555555560687 ) ) ;
#9177 = CARTESIAN_POINT ( 'NONE',  ( 3.070933240276034759, 59.99999999999999289, -32.85680095556730862 ) ) ;
#9178 = DIRECTION ( 'NONE',  ( -0.9860132971832694659, -1.788557213313974350E-28, 0.1666666666666658247 ) ) ;
#9179 = CARTESIAN_POINT ( 'NONE',  ( 29.82695610816121956, 54.99999999999999289, -23.54469556655648077 ) ) ;
#9180 = DIRECTION ( 'NONE',  ( 0.000000000000000000, 0.000000000000000000, 1.000000000000000000 ) ) ;
#9181 = ORIENTED_EDGE ( 'NONE', *, *, #553, .T. ) ;
#9182 = DIRECTION ( 'NONE',  ( -0.9860132971832694659, -1.788557213313974350E-28, 0.1666666666666658247 ) ) ;
#9183 = TOROIDAL_SURFACE ( 'NONE', #6637, 33.00000000000000000, 5.000000000000000000 ) ;
#9184 = VERTEX_POINT ( 'NONE', #4112 ) ;
#9185 = CARTESIAN_POINT ( 'NONE',  ( 9.762153702110021092E-27, 46.00000000000018474, -25.00000000000000000 ) ) ;
#9186 = ORIENTED_EDGE ( 'NONE', *, *, #1073, .F. ) ;
#9187 = CYLINDRICAL_SURFACE ( 'NONE', #2553, 1.500000000000001332 ) ;
#9188 = FACE_OUTER_BOUND ( 'NONE', #3477, .T. ) ;
#9189 = ORIENTED_EDGE ( 'NONE', *, *, #2646, .T. ) ;
#9190 = CIRCLE ( 'NONE', #3339, 26.00000000000006395 ) ;
#9191 = CARTESIAN_POINT ( 'NONE',  ( 32.59762842694625817, 60.99999999999999289, -3.637569555611369854 ) ) ;
#9192 = DIRECTION ( 'NONE',  ( 0.000000000000000000, 1.000000000000000000, 0.000000000000000000 ) ) ;
#9193 = ORIENTED_EDGE ( 'NONE', *, *, #4010, .T. ) ;
#9194 = CARTESIAN_POINT ( 'NONE',  ( 4.687036446413768154, -10.75076954218533132, 38.71946050564961439 ) ) ;
#9195 = ITEM_DEFINED_TRANSFORMATION ( 'NONE', 'NONE', #8703,  #6314 ) ;
#9196 = AXIS2_PLACEMENT_3D ( 'NONE', #9578, #8274, #1453 ) ;
#9197 = ORIENTED_EDGE ( 'NONE', *, *, #1088, .T. ) ;
#9198 = CARTESIAN_POINT ( 'NONE',  ( 1.300000000000000044, 0.000000000000000000, 0.000000000000000000 ) ) ;
#9199 = CARTESIAN_POINT ( 'NONE',  ( -20.44670930779904339, 59.99999999999999289, -25.90235662024527841 ) ) ;
#9200 = CARTESIAN_POINT ( 'NONE',  ( -4.000000000000005329, 28.99999999999997158, 0.000000000000000000 ) ) ;
#9201 = ORIENTED_EDGE ( 'NONE', *, *, #5999, .F. ) ;
#9202 = DIRECTION ( 'NONE',  ( 0.9444444444444316522, 0.000000000000000000, -0.3286710990611269034 ) ) ;
#9203 = ORIENTED_EDGE ( 'NONE', *, *, #761, .F. ) ;
#9204 = EDGE_CURVE ( 'NONE', #6709, #3624, #5584, .T. ) ;
#9205 = DIRECTION ( 'NONE',  ( -0.000000000000000000, -1.000000000000000000, -0.000000000000000000 ) ) ;
#9206 = AXIS2_PLACEMENT_3D ( 'NONE', #8761, #2673, #1109 ) ;
#9207 = LINE ( 'NONE', #8465, #8090 ) ;
#9208 = VECTOR ( 'NONE', #4252, 1000.000000000000000 ) ;
#9209 = ORIENTED_EDGE ( 'NONE', *, *, #6293, .F. ) ;
#9210 = CARTESIAN_POINT ( 'NONE',  ( -3.584397025509258761, -8.971624701663312607, 39.30274302901151628 ) ) ;
#9211 = EDGE_LOOP ( 'NONE', ( #7392, #4506, #1727, #5595, #6824 ) ) ;
#9212 = ORIENTED_EDGE ( 'NONE', *, *, #1307, .F. ) ;
#9213 = CARTESIAN_POINT ( 'NONE',  ( -4.439212511098975966, -5.714671299323741849, 38.81770112249359528 ) ) ;
#9214 = ADVANCED_FACE ( 'NONE', ( #1045 ), #1779, .F. ) ;
#9215 = EDGE_CURVE ( 'NONE', #5855, #1789, #5448, .T. ) ;
#9216 = EDGE_CURVE ( 'NONE', #3216, #6218, #8460, .T. ) ;
#9217 = EDGE_CURVE ( 'NONE', #7758, #7231, #8175, .T. ) ;
#9218 = CARTESIAN_POINT ( 'NONE',  ( 5.562309845534588959, 69.99999999999998579, -33.06426808735054124 ) ) ;
#9219 = EDGE_LOOP ( 'NONE', ( #9028, #3109, #5400, #6336 ) ) ;
#9220 = DIRECTION ( 'NONE',  ( 0.000000000000000000, 0.000000000000000000, 1.000000000000000000 ) ) ;
#9221 = FACE_BOUND ( 'NONE', #4212, .T. ) ;
#9222 = ORIENTED_EDGE ( 'NONE', *, *, #2081, .F. ) ;
#9223 = DIRECTION ( 'NONE',  ( -1.735493991486225972E-29, 6.508102468073347395E-30, 1.000000000000000000 ) ) ;
#9224 = CARTESIAN_POINT ( 'NONE',  ( 3.516611797194487465, 59.70849920474193340, -34.51129295977867883 ) ) ;
#9225 = DIRECTION ( 'NONE',  ( -0.1666666666666658525, -3.897465909857536228E-29, -0.9860132971832695770 ) ) ;
#9226 =( NAMED_UNIT ( * ) SI_UNIT ( $, .STERADIAN. ) SOLID_ANGLE_UNIT ( ) );
#9227 = AXIS2_PLACEMENT_3D ( 'NONE', #3093, #8391, #8938 ) ;
#9228 = DIRECTION ( 'NONE',  ( -0.000000000000000000, 1.000000000000000000, -0.000000000000000000 ) ) ;
#9229 = VERTEX_POINT ( 'NONE', #5639 ) ;
#9230 = CARTESIAN_POINT ( 'NONE',  ( -31.11591804390328164, 61.99999999999999289, 4.904043666719710259 ) ) ;
#9231 = VECTOR ( 'NONE', #9666, 1000.000000000000000 ) ;
#9232 = DIRECTION ( 'NONE',  ( -0.9444444444444404230, -1.387778780781445281E-15, 0.3286710990611014238 ) ) ;
#9233 = VERTEX_POINT ( 'NONE', #9389 ) ;
#9234 = CARTESIAN_POINT ( 'NONE',  ( 0.000000000000000000, 30.00000000000000000, 0.000000000000000000 ) ) ;
#9235 = CARTESIAN_POINT ( 'NONE',  ( 36.28089590215267179, 61.98637676474528746, 8.721193672020515208 ) ) ;
#9236 = VERTEX_POINT ( 'NONE', #948 ) ;
#9237 = VECTOR ( 'NONE', #7521, 1000.000000000000000 ) ;
#9238 = CONICAL_SURFACE ( 'NONE', #2588, 10.00000000000001421, 0.07734202994352787353 ) ;
#9239 = CARTESIAN_POINT ( 'NONE',  ( 0.000000000000000000, 30.00000000000000000, 29.00000000000000355 ) ) ;
#9240 = CARTESIAN_POINT ( 'NONE',  ( 3.332326962091927580, 62.00000000000000711, -36.97859170863235789 ) ) ;
#9241 = ORIENTED_EDGE ( 'NONE', *, *, #649, .F. ) ;
#9242 = VECTOR ( 'NONE', #3367, 1000.000000000000000 ) ;
#9243 = CARTESIAN_POINT ( 'NONE',  ( 0.000000000000000000, 59.99999999999999289, 0.000000000000000000 ) ) ;
#9244 = EDGE_CURVE ( 'NONE', #6026, #2210, #3962, .T. ) ;
#9245 = CIRCLE ( 'NONE', #5773, 2.499999999999998668 ) ;
#9246 = EDGE_LOOP ( 'NONE', ( #5190, #5253, #402, #1399 ) ) ;
#9247 = FACE_OUTER_BOUND ( 'NONE', #3927, .T. ) ;
#9248 = CARTESIAN_POINT ( 'NONE',  ( -25.23917843705063646, 29.66524321760768501, 4.665243217607709880 ) ) ;
#9249 = DIRECTION ( 'NONE',  ( -0.000000000000000000, -1.000000000000000000, -0.000000000000000000 ) ) ;
#9250 = CARTESIAN_POINT ( 'NONE',  ( 7.848671329280706210, 59.99999999999999289, -32.05305536707737701 ) ) ;
#9251 = ORIENTED_EDGE ( 'NONE', *, *, #3957, .T. ) ;
#9252 = VECTOR ( 'NONE', #260, 1000.000000000000000 ) ;
#9253 = DIRECTION ( 'NONE',  ( -0.7849198975831886971, -1.387778780781445281E-15, 0.6195972517514877209 ) ) ;
#9254 = CARTESIAN_POINT ( 'NONE',  ( -3.582198172489065691, -6.047248247680749422, 43.67305511344584801 ) ) ;
#9255 = AXIS2_PLACEMENT_3D ( 'NONE', #4803, #4064, #2413 ) ;
#9256 = ORIENTED_EDGE ( 'NONE', *, *, #223, .T. ) ;
#9257 = ORIENTED_EDGE ( 'NONE', *, *, #8799, .T. ) ;
#9258 = FACE_OUTER_BOUND ( 'NONE', #4644, .T. ) ;
#9259 = VERTEX_POINT ( 'NONE', #9250 ) ;
#9260 = ORIENTED_EDGE ( 'NONE', *, *, #810, .T. ) ;
#9261 = CARTESIAN_POINT ( 'NONE',  ( -6.118192406390955185, -4.621831477418986367, 43.03401398244064069 ) ) ;
#9262 = EDGE_CURVE ( 'NONE', #285, #3751, #2464, .T. ) ;
#9263 = EDGE_CURVE ( 'NONE', #880, #5898, #3732, .T. ) ;
#9264 = CYLINDRICAL_SURFACE ( 'NONE', #8881, 2.500000000000002220 ) ;
#9265 = AXIS2_PLACEMENT_3D ( 'NONE', #9612, #8781, #7290 ) ;
#9266 = ORIENTED_EDGE ( 'NONE', *, *, #8118, .T. ) ;
#9267 = DIRECTION ( 'NONE',  ( 0.000000000000000000, 0.000000000000000000, -1.000000000000000000 ) ) ;
#9268 = EDGE_CURVE ( 'NONE', #7767, #7682, #435, .T. ) ;
#9269 = ORIENTED_EDGE ( 'NONE', *, *, #4744, .T. ) ;
#9270 = DIRECTION ( 'NONE',  ( -0.000000000000000000, -1.000000000000000000, -0.000000000000000000 ) ) ;
#9271 = ADVANCED_FACE ( 'NONE', ( #600 ), #4216, .T. ) ;
#9272 = CARTESIAN_POINT ( 'NONE',  ( 3.339929591309186652, 59.80724097760847968, -34.22175998453048607 ) ) ;
#9273 = DIRECTION ( 'NONE',  ( 8.659560562354962440E-17, 0.7071067811865451302, -0.7071067811865500152 ) ) ;
#9274 = FACE_OUTER_BOUND ( 'NONE', #7094, .T. ) ;
#9275 = CARTESIAN_POINT ( 'NONE',  ( -5.562309845534584518, 69.99999999999998579, 35.56426808735054834 ) ) ;
#9276 = B_SPLINE_CURVE_WITH_KNOTS ( 'NONE', 3,
 ( #5219, #2182, #5372, #8425, #5424, #8382, #3891, #4637, #8973, #6039, #1614, #5951, #6100, #7592, #8279, #1659, #6884, #3330, #3836, #7441, #8226, #6832, #7489, #5266 ),
 .UNSPECIFIED., .F., .F.,
 ( 4, 2, 2, 2, 2, 2, 2, 2, 2, 2, 2, 4 ),
 ( 0.06349434409688703429, 0.06548129692158807802, 0.06647477333393859988, 0.06746824974628912175, 0.06945520257099015160, 0.07144215539569119533, 0.07342910822039223906, 0.07442258463274276092, 0.07541606104509328279, 0.07640953745744380465, 0.07740301386979431264, 0.07938996669449535637 ),
 .UNSPECIFIED. ) ;
#9277 = DIRECTION ( 'NONE',  ( -0.000000000000000000, 1.000000000000000000, -0.000000000000000000 ) ) ;
#9278 = EDGE_CURVE ( 'NONE', #8311, #7524, #2194, .T. ) ;
#9279 = CARTESIAN_POINT ( 'NONE',  ( -8.216777476527294510, 52.00000000000031974, -23.61111111111111427 ) ) ;
#9280 = EDGE_CURVE ( 'NONE', #5111, #326, #3893, .T. ) ;
#9281 = DIRECTION ( 'NONE',  ( -1.820952055660014662E-28, -1.000000000000000000, -7.038118388768679669E-30 ) ) ;
#9282 = ADVANCED_FACE ( 'NONE', ( #9188 ), #5927, .T. ) ;
#9283 = ORIENTED_EDGE ( 'NONE', *, *, #4261, .F. ) ;
#9284 = CARTESIAN_POINT ( 'NONE',  ( 7.214865095668090866, 61.84561525624321376, -37.26328141369675251 ) ) ;
#9285 = CARTESIAN_POINT ( 'NONE',  ( 37.55900191124520404, 61.85658167520826822, 5.210294541070858543 ) ) ;
#9286 = ORIENTED_EDGE ( 'NONE', *, *, #7837, .F. ) ;
#9287 = FACE_OUTER_BOUND ( 'NONE', #8783, .T. ) ;
#9288 = CARTESIAN_POINT ( 'NONE',  ( -37.19753653653384617, 61.85638901966269287, -7.362986651992473597 ) ) ;
#9289 = CARTESIAN_POINT ( 'NONE',  ( 5.894973159897614501, -10.18605400909195602, 38.56045930014798984 ) ) ;
#9290 = DIRECTION ( 'NONE',  ( -0.000000000000000000, -0.5000000000000002220, 0.8660254037844384856 ) ) ;
#9291 = ORIENTED_EDGE ( 'NONE', *, *, #952, .T. ) ;
#9292 = CYLINDRICAL_SURFACE ( 'NONE', #1339, 34.49999999999999289 ) ;
#9293 = ORIENTED_EDGE ( 'NONE', *, *, #1489, .T. ) ;
#9294 = DIRECTION ( 'NONE',  ( 0.9860132971832693549, 1.788557213313974126E-28, -0.1666666666666657970 ) ) ;
#9295 = ORIENTED_EDGE ( 'NONE', *, *, #5529, .T. ) ;
#9296 = DIRECTION ( 'NONE',  ( -1.000000000000000000, 0.000000000000000000, -3.083952846180987322E-15 ) ) ;
#9297 = EDGE_CURVE ( 'NONE', #6014, #7004, #8641, .T. ) ;
#9298 = DIRECTION ( 'NONE',  ( 0.000000000000000000, 0.000000000000000000, 1.000000000000000000 ) ) ;
#9299 = VERTEX_POINT ( 'NONE', #2454 ) ;
#9300 = CARTESIAN_POINT ( 'NONE',  ( -35.54672840350796292, 58.97502204235875922, -5.902312647278756153 ) ) ;
#9301 = VERTEX_POINT ( 'NONE', #2402 ) ;
#9302 = CARTESIAN_POINT ( 'NONE',  ( -33.06426808735053413, 59.89212256466219486, -8.062309845534585406 ) ) ;
#9303 = CIRCLE ( 'NONE', #783, 33.00000000000000711 ) ;
#9304 = AXIS2_PLACEMENT_3D ( 'NONE', #8866, #1900, #2784 ) ;
#9305 = ORIENTED_EDGE ( 'NONE', *, *, #7087, .F. ) ;
#9306 = CARTESIAN_POINT ( 'NONE',  ( -9.978207696992249964, 4.056654655798920928, 37.86436474176541367 ) ) ;
#9307 = DIRECTION ( 'NONE',  ( 1.000000000000000000, 0.000000000000000000, 1.079383496163345602E-14 ) ) ;
#9308 = DIRECTION ( 'NONE',  ( 0.000000000000000000, 0.000000000000000000, 1.000000000000000000 ) ) ;
#9309 = ORIENTED_EDGE ( 'NONE', *, *, #7273, .F. ) ;
#9310 = DIRECTION ( 'NONE',  ( -1.000000000000000000, 0.000000000000000000, 0.000000000000000000 ) ) ;
#9311 = EDGE_CURVE ( 'NONE', #7141, #5164, #9724, .T. ) ;
#9312 = LINE ( 'NONE', #5515, #9681 ) ;
#9313 = CARTESIAN_POINT ( 'NONE',  ( 3.976301758542440279, 59.47750853442942542, -35.00401529666653033 ) ) ;
#9314 = CARTESIAN_POINT ( 'NONE',  ( 23.54759692749571443, 59.99999999999999289, -18.58791755254457811 ) ) ;
#9315 = CARTESIAN_POINT ( 'NONE',  ( 6.000000000000001776, -15.00000000000000000, -31.00000000000000711 ) ) ;
#9316 = CARTESIAN_POINT ( 'NONE',  ( 1.300000000000000044, -0.7216878364870318308, 1.250000000000000000 ) ) ;
#9317 = CIRCLE ( 'NONE', #5060, 2.499999999999998668 ) ;
#9318 = DIRECTION ( 'NONE',  ( -1.820952055660014662E-28, -1.000000000000000000, -7.038118388768679669E-30 ) ) ;
#9319 = MECHANICAL_DESIGN_GEOMETRIC_PRESENTATION_REPRESENTATION (  '', ( #5848 ), #6781 ) ;
#9320 = CARTESIAN_POINT ( 'NONE',  ( -28.33333333333344939, 59.99999999999999289, 9.860132971832396009 ) ) ;
#9321 = ORIENTED_EDGE ( 'NONE', *, *, #412, .F. ) ;
#9322 = CARTESIAN_POINT ( 'NONE',  ( 1.203012880462043003E-26, 59.00000000000029843, -37.00000000000000711 ) ) ;
#9323 = ORIENTED_EDGE ( 'NONE', *, *, #3114, .F. ) ;
#9324 = CARTESIAN_POINT ( 'NONE',  ( -33.06426808735054124, 69.99999999999998579, -8.062309845534583630 ) ) ;
#9325 = DIRECTION ( 'NONE',  ( 0.000000000000000000, 0.000000000000000000, 1.000000000000000000 ) ) ;
#9326 = ORIENTED_EDGE ( 'NONE', *, *, #4051, .F. ) ;
#9327 = LINE ( 'NONE', #7798, #2740 ) ;
#9328 = EDGE_CURVE ( 'NONE', #7653, #2998, #4790, .T. ) ;
#9329 = CARTESIAN_POINT ( 'NONE',  ( 0.000000000000000000, 39.99999999999999289, 0.000000000000000000 ) ) ;
#9330 = EDGE_CURVE ( 'NONE', #179, #2965, #6204, .T. ) ;
#9331 = EDGE_CURVE ( 'NONE', #960, #7928, #5433, .T. ) ;
#9332 = DIRECTION ( 'NONE',  ( 0.000000000000000000, -1.000000000000000000, 0.000000000000000000 ) ) ;
#9333 = CARTESIAN_POINT ( 'NONE',  ( 0.000000000000000000, 1.000000000000014655, 0.000000000000000000 ) ) ;
#9334 = ORIENTED_EDGE ( 'NONE', *, *, #249, .T. ) ;
#9335 = DIRECTION ( 'NONE',  ( -1.000000000000000000, 0.000000000000000000, 2.168404344971006649E-16 ) ) ;
#9336 = ORIENTED_EDGE ( 'NONE', *, *, #1694, .T. ) ;
#9337 = DIRECTION ( 'NONE',  ( 0.000000000000000000, 0.000000000000000000, 1.000000000000000000 ) ) ;
#9338 = ORIENTED_EDGE ( 'NONE', *, *, #2969, .F. ) ;
#9339 = CARTESIAN_POINT ( 'NONE',  ( 0.000000000000000000, 28.99999999999997158, 29.00000000000000355 ) ) ;
#9340 = CIRCLE ( 'NONE', #671, 4.500000000000005329 ) ;
#9341 = VERTEX_POINT ( 'NONE', #6303 ) ;
#9342 = CARTESIAN_POINT ( 'NONE',  ( -8.216777476527294510, 44.50000000000019185, -23.61111111111111427 ) ) ;
#9343 = EDGE_CURVE ( 'NONE', #6468, #8122, #3949, .T. ) ;
#9344 = LINE ( 'NONE', #7110, #4349 ) ;
#9345 = VECTOR ( 'NONE', #3951, 1000.000000000000000 ) ;
#9346 = VERTEX_POINT ( 'NONE', #3248 ) ;
#9347 = CARTESIAN_POINT ( 'NONE',  ( 18.58791755254457811, 59.99999999999999289, 23.54759692749571443 ) ) ;
#9348 = EDGE_LOOP ( 'NONE', ( #959, #4993, #6210, #8098 ) ) ;
#9349 = VERTEX_POINT ( 'NONE', #7096 ) ;
#9350 = CARTESIAN_POINT ( 'NONE',  ( 35.90836395996004171, 39.99999999999999289, 12.43339847825378186 ) ) ;
#9351 = ORIENTED_EDGE ( 'NONE', *, *, #9263, .F. ) ;
#9352 = CARTESIAN_POINT ( 'NONE',  ( -5.263670707606620702, -5.244400598322866536, 38.72935084317680321 ) ) ;
#9353 = AXIS2_PLACEMENT_3D ( 'NONE', #5318, #1749, #9120 ) ;
#9354 = VECTOR ( 'NONE', #9575, 1000.000000000000000 ) ;
#9355 = CARTESIAN_POINT ( 'NONE',  ( 0.000000000000000000, 54.99999999999999289, 0.000000000000000000 ) ) ;
#9356 = LINE ( 'NONE', #6384, #3998 ) ;
#9357 = ORIENTED_EDGE ( 'NONE', *, *, #6475, .T. ) ;
#9358 = DIRECTION ( 'NONE',  ( 0.000000000000000000, 0.000000000000000000, 1.000000000000000000 ) ) ;
#9359 = EDGE_LOOP ( 'NONE', ( #2290, #9417, #2527, #7379, #9047 ) ) ;
#9360 = CARTESIAN_POINT ( 'NONE',  ( -10.00000000000001421, 3.294852476641298100, 184.6745183374407020 ) ) ;
#9361 = DIRECTION ( 'NONE',  ( -1.820952055660014662E-28, -1.000000000000000000, -7.038118388768679669E-30 ) ) ;
#9362 = DIRECTION ( 'NONE',  ( -0.000000000000000000, 1.000000000000000000, -0.000000000000000000 ) ) ;
#9363 = CARTESIAN_POINT ( 'NONE',  ( 12.42372165054948141, -2.086834094042897103, 36.96875360800631682 ) ) ;
#9364 = DIRECTION ( 'NONE',  ( 0.000000000000000000, -1.000000000000000000, 0.000000000000000000 ) ) ;
#9365 = PLANE ( 'NONE',  #6536 ) ;
#9366 = CARTESIAN_POINT ( 'NONE',  ( -8.545448575588375562, -1.756255516286720374E-27, -24.55555555555558911 ) ) ;
#9367 = CARTESIAN_POINT ( 'NONE',  ( 29.00000000000000355, 30.00000000000000000, -4.000000000000007105 ) ) ;
#9368 = VERTEX_POINT ( 'NONE', #5573 ) ;
#9369 = VECTOR ( 'NONE', #4737, 1000.000000000000000 ) ;
#9370 = DIRECTION ( 'NONE',  ( -1.000000000000000000, -0.000000000000000000, 1.084202172485503448E-16 ) ) ;
#9371 = CARTESIAN_POINT ( 'NONE',  ( -2.094888803305880518E-13, 39.99999999999999289, 30.00000000000000711 ) ) ;
#9372 = ORIENTED_EDGE ( 'NONE', *, *, #825, .T. ) ;
#9373 = DIRECTION ( 'NONE',  ( -0.000000000000000000, 1.000000000000000000, -0.000000000000000000 ) ) ;
#9374 = CARTESIAN_POINT ( 'NONE',  ( 37.19753653653384617, 61.85638901966269287, 7.362986651992473597 ) ) ;
#9375 = ORIENTED_EDGE ( 'NONE', *, *, #1071, .F. ) ;
#9376 = CARTESIAN_POINT ( 'NONE',  ( -12.93864508289175141, -0.2176600089833630181, 36.79137408646710838 ) ) ;
#9377 = CARTESIAN_POINT ( 'NONE',  ( 5.137569555611264605, 60.99999999999999289, 32.59762842694627949 ) ) ;
#9378 = AXIS2_PLACEMENT_3D ( 'NONE', #3188, #886, #6890 ) ;
#9379 = VECTOR ( 'NONE', #6599, 1000.000000000000000 ) ;
#9380 = CARTESIAN_POINT ( 'NONE',  ( -37.01190402608325059, 62.00000000000000711, -3.384896555618068348 ) ) ;
#9381 = DIRECTION ( 'NONE',  ( -0.000000000000000000, -1.000000000000000000, -0.000000000000000000 ) ) ;
#9382 = DIRECTION ( 'NONE',  ( 0.000000000000000000, 0.000000000000000000, 1.000000000000000000 ) ) ;
#9383 = AXIS2_PLACEMENT_3D ( 'NONE', #2153, #7359, #6510 ) ;
#9384 = EDGE_CURVE ( 'NONE', #7724, #5165, #1682, .T. ) ;
#9385 = AXIS2_PLACEMENT_3D ( 'NONE', #5758, #4833, #6440 ) ;
#9386 = VERTEX_POINT ( 'NONE', #204 ) ;
#9387 = CARTESIAN_POINT ( 'NONE',  ( 0.000000000000000000, 59.99999999999999289, -30.00000000000000711 ) ) ;
#9388 = ORIENTED_EDGE ( 'NONE', *, *, #4213, .F. ) ;
#9389 = CARTESIAN_POINT ( 'NONE',  ( -4.000000000000005329, 0.000000000000000000, -29.00000000000000355 ) ) ;
#9390 = EDGE_CURVE ( 'NONE', #3249, #7030, #1679, .T. ) ;
#9391 = VERTEX_POINT ( 'NONE', #4700 ) ;
#9392 = PLANE ( 'NONE',  #206 ) ;
#9393 = AXIS2_PLACEMENT_3D ( 'NONE', #6009, #1683, #9043 ) ;
#9394 = AXIS2_PLACEMENT_3D ( 'NONE', #3610, #5833, #7370 ) ;
#9395 = CARTESIAN_POINT ( 'NONE',  ( 8.677469957431129860E-27, 45.50000000000019185, -24.09806918451535651 ) ) ;
#9396 = CIRCLE ( 'NONE', #6070, 19.00000000000000355 ) ;
#9397 = AXIS2_PLACEMENT_3D ( 'NONE', #83, #6135, #6093 ) ;
#9398 = DIRECTION ( 'NONE',  ( 0.000000000000000000, 0.000000000000000000, 1.000000000000000000 ) ) ;
#9399 = CARTESIAN_POINT ( 'NONE',  ( -33.06426808735054124, 60.99999999999999289, -10.06230984553459251 ) ) ;
#9400 = VERTEX_POINT ( 'NONE', #1030 ) ;
#9401 = EDGE_LOOP ( 'NONE', ( #2436, #7912, #3553, #3105, #8025 ) ) ;
#9402 = DIRECTION ( 'NONE',  ( 0.000000000000000000, 0.000000000000000000, -1.000000000000000000 ) ) ;
#9403 = EDGE_CURVE ( 'NONE', #1842, #6584, #3997, .T. ) ;
#9404 = AXIS2_PLACEMENT_3D ( 'NONE', #6392, #2580, #8575 ) ;
#9405 = ORIENTED_EDGE ( 'NONE', *, *, #1905, .T. ) ;
#9406 = CARTESIAN_POINT ( 'NONE',  ( 0.000000000000000000, 0.000000000000000000, 0.000000000000000000 ) ) ;
#9407 = ORIENTED_EDGE ( 'NONE', *, *, #1548, .T. ) ;
#9408 = AXIS2_PLACEMENT_3D ( 'NONE', #701, #854, #3054 ) ;
#9409 = VERTEX_POINT ( 'NONE', #343 ) ;
#9410 = EDGE_CURVE ( 'NONE', #1736, #7319, #3496, .T. ) ;
#9411 = CARTESIAN_POINT ( 'NONE',  ( -12.44909004914269168, -1.994056636296514196, 36.96012135774385143 ) ) ;
#9412 = PLANE ( 'NONE',  #5610 ) ;
#9413 = DIRECTION ( 'NONE',  ( 0.000000000000000000, 0.000000000000000000, 1.000000000000000000 ) ) ;
#9414 = AXIS2_PLACEMENT_3D ( 'NONE', #1469, #7505, #8443 ) ;
#9415 = ORIENTED_EDGE ( 'NONE', *, *, #4496, .T. ) ;
#9416 = CARTESIAN_POINT ( 'NONE',  ( 0.000000000000000000, 0.000000000000000000, 0.000000000000000000 ) ) ;
#9417 = ORIENTED_EDGE ( 'NONE', *, *, #5947, .T. ) ;
#9418 = CARTESIAN_POINT ( 'NONE',  ( -9.860132971832692661, 59.99999999999999289, -28.33333333333334281 ) ) ;
#9419 = VERTEX_POINT ( 'NONE', #6989 ) ;
#9420 = CARTESIAN_POINT ( 'NONE',  ( -32.85680095556730862, 59.99999999999999289, -3.070933240276025877 ) ) ;
#9421 = DIRECTION ( 'NONE',  ( 0.000000000000000000, 0.000000000000000000, 1.000000000000000000 ) ) ;
#9422 = AXIS2_PLACEMENT_3D ( 'NONE', #3397, #630, #2097 ) ;
#9423 = DIRECTION ( 'NONE',  ( -0.000000000000000000, 1.000000000000000000, -0.000000000000000000 ) ) ;
#9424 = FACE_OUTER_BOUND ( 'NONE', #1056, .T. ) ;
#9425 = DIRECTION ( 'NONE',  ( -0.000000000000000000, -1.000000000000000000, -0.000000000000000000 ) ) ;
#9426 = LINE ( 'NONE', #2639, #879 ) ;
#9427 = EDGE_CURVE ( 'NONE', #7406, #3754, #4686, .T. ) ;
#9428 = VERTEX_POINT ( 'NONE', #9433 ) ;
#9429 = LINE ( 'NONE', #4734, #6979 ) ;
#9430 = CARTESIAN_POINT ( 'NONE',  ( 0.6802059239249094169, 13.27724345761031799, 43.99097674794369794 ) ) ;
#9431 = ORIENTED_EDGE ( 'NONE', *, *, #6549, .T. ) ;
#9432 = DIRECTION ( 'NONE',  ( 0.000000000000000000, 1.000000000000000000, 0.000000000000000000 ) ) ;
#9433 = CARTESIAN_POINT ( 'NONE',  ( -8.545448575588393325, 50.50000000000031974, -24.55555555555563529 ) ) ;
#9434 = ORIENTED_EDGE ( 'NONE', *, *, #7997, .F. ) ;
#9435 = CARTESIAN_POINT ( 'NONE',  ( 0.000000000000000000, 59.99999999999999289, -30.00000000000000711 ) ) ;
#9436 = FACE_OUTER_BOUND ( 'NONE', #9102, .T. ) ;
#9437 = CARTESIAN_POINT ( 'NONE',  ( -36.64076086657617282, 61.94822636785970360, -8.307112375470062204 ) ) ;
#9438 = CARTESIAN_POINT ( 'NONE',  ( 31.00000000000000711, -10.00000000000000533, -6.000000000000006217 ) ) ;
#9439 = ORIENTED_EDGE ( 'NONE', *, *, #8666, .T. ) ;
#9440 = LINE ( 'NONE', #2653, #2587 ) ;
#9441 = CARTESIAN_POINT ( 'NONE',  ( -8.825403668520980460, -15.00000000000000000, 36.98508877022077002 ) ) ;
#9442 = EDGE_CURVE ( 'NONE', #6031, #7876, #9523, .T. ) ;
#9443 = VERTEX_POINT ( 'NONE', #2644 ) ;
#9444 = MANIFOLD_SOLID_BREP ( 'Cut-Extrude5', #3898 ) ;
#9445 = CARTESIAN_POINT ( 'NONE',  ( 33.06426808735054124, 49.99999999999999289, 3.062309845534584074 ) ) ;
#9446 = FACE_OUTER_BOUND ( 'NONE', #9489, .T. ) ;
#9447 = ADVANCED_FACE ( 'NONE', ( #2794 ), #8690, .F. ) ;
#9448 = CARTESIAN_POINT ( 'NONE',  ( 4.458695940319988615, 12.25186834038896677, 43.49095922549461335 ) ) ;
#9449 = CARTESIAN_POINT ( 'NONE',  ( 1.300000000000000044, 0.7216878364870328300, 1.250000000000000000 ) ) ;
#9450 = LINE ( 'NONE', #9399, #1259 ) ;
#9451 = ORIENTED_EDGE ( 'NONE', *, *, #8819, .F. ) ;
#9452 = CARTESIAN_POINT ( 'NONE',  ( 1.084683744678891232E-26, 53.50000000000031264, -25.00000000000000000 ) ) ;
#9453 = ORIENTED_EDGE ( 'NONE', *, *, #1898, .F. ) ;
#9454 = PLANE ( 'NONE',  #5137 ) ;
#9455 = ORIENTED_EDGE ( 'NONE', *, *, #5225, .T. ) ;
#9456 = CARTESIAN_POINT ( 'NONE',  ( -10.82069016047256227, -5.434853743389174596, 37.46967153039774701 ) ) ;
#9457 = CARTESIAN_POINT ( 'NONE',  ( 0.000000000000000000, 30.00000000000000000, 39.00000000000002132 ) ) ;
#9458 = DIRECTION ( 'NONE',  ( 1.000000000000000000, 0.000000000000000000, -1.224646799147353207E-16 ) ) ;
#9459 = EDGE_CURVE ( 'NONE', #3643, #5005, #4531, .T. ) ;
#9460 = EDGE_CURVE ( 'NONE', #77, #2117, #4882, .T. ) ;
#9461 = EDGE_CURVE ( 'NONE', #5230, #2792, #4936, .T. ) ;
#9462 = VECTOR ( 'NONE', #3527, 1000.000000000000000 ) ;
#9463 = ORIENTED_EDGE ( 'NONE', *, *, #2015, .F. ) ;
#9464 = DIRECTION ( 'NONE',  ( 0.000000000000000000, 0.000000000000000000, -1.000000000000000000 ) ) ;
#9465 = ORIENTED_EDGE ( 'NONE', *, *, #4430, .F. ) ;
#9466 = DIRECTION ( 'NONE',  ( 1.735493991486224571E-29, 0.000000000000000000, -1.000000000000000000 ) ) ;
#9467 = DIRECTION ( 'NONE',  ( 0.000000000000000000, 0.000000000000000000, 1.000000000000000000 ) ) ;
#9468 = CYLINDRICAL_SURFACE ( 'NONE', #5387, 2.500000000000002220 ) ;
#9469 = DIRECTION ( 'NONE',  ( 0.000000000000000000, 1.000000000000000000, 0.000000000000000000 ) ) ;
#9470 = DIRECTION ( 'NONE',  ( 0.000000000000000000, 0.000000000000000000, 1.000000000000000000 ) ) ;
#9471 = B_SPLINE_CURVE_WITH_KNOTS ( 'NONE', 3,
 ( #7719, #1152, #228, #2469, #5505, #8511, #1742, #4764, #7768, #1003, #1787, #7012, #276, #9300, #2513, #4813, #7821, #6467, #1389, #6658, #9683, #2909, #5926, #9593, #5098, #6571, #563, #1981, #5791, #8105, #5151, #5004 ),
 .UNSPECIFIED., .F., .F.,
 ( 4, 2, 2, 2, 2, 2, 2, 2, 2, 2, 2, 2, 2, 2, 2, 4 ),
 ( 0.001042552523569530588, 0.002052900844284173687, 0.002558075004641498489, 0.003063249164998823292, 0.003568423325356147660, 0.004073597485713472896, 0.004578771646070796397, 0.005083945806428121633, 0.005589119966785446869, 0.006094294127142772105, 0.006599468287500097341, 0.007104642447857422577, 0.007609816608214747813, 0.008114990768572073049, 0.008620164928929398285, 0.009125339089286721786 ),
 .UNSPECIFIED. ) ;
#9472 = ORIENTED_EDGE ( 'NONE', *, *, #8073, .F. ) ;
#9473 = CARTESIAN_POINT ( 'NONE',  ( 31.00000000000000711, -10.00000000000000533, 6.000000000000000000 ) ) ;
#9474 = DIRECTION ( 'NONE',  ( 0.000000000000000000, -1.000000000000000000, 0.000000000000000000 ) ) ;
#9475 = VERTEX_POINT ( 'NONE', #1960 ) ;
#9476 = LINE ( 'NONE', #6638, #9354 ) ;
#9477 = PRODUCT_DEFINITION ( 'UNKNOWN', '', #500, #1148 ) ;
#9478 = CARTESIAN_POINT ( 'NONE',  ( 33.06426808735054124, 61.99999999999999289, 10.06230984553459251 ) ) ;
#9479 = CARTESIAN_POINT ( 'NONE',  ( 0.000000000000000000, 0.000000000000000000, 0.000000000000000000 ) ) ;
#9480 = DIRECTION ( 'NONE',  ( -0.000000000000000000, 1.000000000000000000, -0.000000000000000000 ) ) ;
#9481 = VERTEX_POINT ( 'NONE', #7351 ) ;
#9482 = FACE_BOUND ( 'NONE', #57, .T. ) ;
#9483 = CARTESIAN_POINT ( 'NONE',  ( -3.216413334743783103, -15.00000000000062883, 36.77513389234219687 ) ) ;
#9484 = EDGE_LOOP ( 'NONE', ( #1859, #6769, #8711, #8416 ) ) ;
#9485 = CARTESIAN_POINT ( 'NONE',  ( 0.000000000000000000, 59.99999999999999289, -27.99999999999999289 ) ) ;
#9486 = LINE ( 'NONE', #313, #725 ) ;
#9487 = CARTESIAN_POINT ( 'NONE',  ( 2.766011525709246577, 12.93636287564932807, 38.93656662069780339 ) ) ;
#9488 = DIRECTION ( 'NONE',  ( 1.000000000000000000, 0.000000000000000000, 0.000000000000000000 ) ) ;
#9489 = EDGE_LOOP ( 'NONE', ( #1721, #5649, #8793, #5293 ) ) ;
#9490 = CARTESIAN_POINT ( 'NONE',  ( 0.000000000000000000, 59.99999999999999289, 0.000000000000000000 ) ) ;
#9491 = ORIENTED_EDGE ( 'NONE', *, *, #2991, .T. ) ;
#9492 = CARTESIAN_POINT ( 'NONE',  ( 33.23540996127940872, 59.98874451312625666, 3.062309845534584074 ) ) ;
#9493 = ORIENTED_EDGE ( 'NONE', *, *, #7818, .T. ) ;
#9494 = ORIENTED_EDGE ( 'NONE', *, *, #1722, .T. ) ;
#9495 = EDGE_CURVE ( 'NONE', #2517, #9574, #8828, .T. ) ;
#9496 = CARTESIAN_POINT ( 'NONE',  ( -7.023314015493160589, 16.04054292710173257, 38.36414130246328114 ) ) ;
#9497 = DIRECTION ( 'NONE',  ( 0.000000000000000000, 0.000000000000000000, 1.000000000000000000 ) ) ;
#9498 = VECTOR ( 'NONE', #558, 1000.000000000000000 ) ;
#9499 = LINE ( 'NONE', #5555, #8566 ) ;
#9500 = ORIENTED_EDGE ( 'NONE', *, *, #4510, .F. ) ;
#9501 = ORIENTED_EDGE ( 'NONE', *, *, #3291, .F. ) ;
#9502 = CARTESIAN_POINT ( 'NONE',  ( 6.000000000000001776, -10.00000000000000533, -31.00000000000000711 ) ) ;
#9503 = EDGE_LOOP ( 'NONE', ( #9197, #7074, #5971, #7263 ) ) ;
#9504 = ORIENTED_EDGE ( 'NONE', *, *, #8054, .T. ) ;
#9505 = CARTESIAN_POINT ( 'NONE',  ( 33.06426808735054124, 60.99999999999999289, 10.06230984553459251 ) ) ;
#9506 = AXIS2_PLACEMENT_3D ( 'NONE', #792, #3803, #9096 ) ;
#9507 = AXIS2_PLACEMENT_3D ( 'NONE', #4546, #7452, #4 ) ;
#9508 = EDGE_CURVE ( 'NONE', #9475, #9233, #6553, .T. ) ;
#9509 = ADVANCED_FACE ( 'NONE', ( #4345 ), #1178, .F. ) ;
#9510 = CARTESIAN_POINT ( 'NONE',  ( -28.37252191822216218, 30.00000000000000000, -5.999999999999996447 ) ) ;
#9511 = CARTESIAN_POINT ( 'NONE',  ( 5.423418723394456162E-28, -2.066522830327504070E-28, -26.00000000000015987 ) ) ;
#9512 = LINE ( 'NONE', #7188, #5684 ) ;
#9513 = EDGE_CURVE ( 'NONE', #9349, #6799, #548, .T. ) ;
#9514 = DIRECTION ( 'NONE',  ( 0.000000000000000000, 0.000000000000000000, -1.000000000000000000 ) ) ;
#9515 = AXIS2_PLACEMENT_3D ( 'NONE', #2131, #2213, #2080 ) ;
#9516 = B_SPLINE_CURVE_WITH_KNOTS ( 'NONE', 3,
 ( #6811, #7568, #165, #68 ),
 .UNSPECIFIED., .F., .F.,
 ( 4, 4 ),
 ( 0.000000000000000000, 0.001643226871903046308 ),
 .UNSPECIFIED. ) ;
#9517 = ORIENTED_EDGE ( 'NONE', *, *, #1954, .F. ) ;
#9518 = CARTESIAN_POINT ( 'NONE',  ( -32.89361530837994962, 59.92713194881500982, -8.062309845534583630 ) ) ;
#9519 = CARTESIAN_POINT ( 'NONE',  ( 9.860132971832495485, 59.99999999999999289, 28.33333333333341031 ) ) ;
#9520 = EDGE_CURVE ( 'NONE', #4557, #8890, #1367, .T. ) ;
#9521 = VERTEX_POINT ( 'NONE', #6595 ) ;
#9522 = CARTESIAN_POINT ( 'NONE',  ( -8.216777476527274970, 47.00000000000034106, -23.61111111111107519 ) ) ;
#9523 = LINE ( 'NONE', #1230, #7519 ) ;
#9524 = ADVANCED_FACE ( 'NONE', ( #6499 ), #9576, .F. ) ;
#9525 = DIRECTION ( 'NONE',  ( 0.000000000000000000, 0.000000000000000000, 1.000000000000000000 ) ) ;
#9526 = CARTESIAN_POINT ( 'NONE',  ( 9.401064979878146488, -6.093490218539241887, 37.92280751639714254 ) ) ;
#9527 = FACE_OUTER_BOUND ( 'NONE', #6593, .T. ) ;
#9528 = CIRCLE ( 'NONE', #1015, 26.00000000000006395 ) ;
#9529 = EDGE_LOOP ( 'NONE', ( #968, #3262, #4163, #2085 ) ) ;
#9530 = DIRECTION ( 'NONE',  ( -0.000000000000000000, -1.000000000000000000, -0.000000000000000000 ) ) ;
#9531 = CARTESIAN_POINT ( 'NONE',  ( -0.5763160496995928250, -9.468987443031627649, 39.52686025307730944 ) ) ;
#9532 = EDGE_LOOP ( 'NONE', ( #5014, #4429, #4535, #2326 ) ) ;
#9533 = AXIS2_PLACEMENT_3D ( 'NONE', #6596, #4543, #46 ) ;
#9534 = AXIS2_PLACEMENT_3D ( 'NONE', #8280, #2940, #5952 ) ;
#9535 = DIRECTION ( 'NONE',  ( 0.000000000000000000, 0.5000000000000002220, -0.8660254037844384856 ) ) ;
#9536 = DIRECTION ( 'NONE',  ( 0.000000000000000000, 0.000000000000000000, 1.000000000000000000 ) ) ;
#9537 = EDGE_CURVE ( 'NONE', #4366, #4372, #6409, .T. ) ;
#9538 = CARTESIAN_POINT ( 'NONE',  ( 8.174139990748312101, 9.098271002114579176, 38.27377497168703968 ) ) ;
#9539 = DIRECTION ( 'NONE',  ( 1.000000000000000000, 0.000000000000000000, 0.000000000000000000 ) ) ;
#9540 = CIRCLE ( 'NONE', #1492, 5.000000000000001776 ) ;
#9541 = EDGE_LOOP ( 'NONE', ( #308, #6666, #4343, #885 ) ) ;
#9542 = FACE_OUTER_BOUND ( 'NONE', #2504, .T. ) ;
#9543 = VERTEX_POINT ( 'NONE', #98 ) ;
#9544 = DIRECTION ( 'NONE',  ( 0.000000000000000000, 0.000000000000000000, 1.000000000000000000 ) ) ;
#9545 = ORIENTED_EDGE ( 'NONE', *, *, #4693, .F. ) ;
#9546 = ORIENTED_EDGE ( 'NONE', *, *, #3777, .T. ) ;
#9547 = LINE ( 'NONE', #2029, #8436 ) ;
#9548 = AXIS2_PLACEMENT_3D ( 'NONE', #4707, #7713, #8505 ) ;
#9549 = CARTESIAN_POINT ( 'NONE',  ( 0.000000000000000000, 59.99999999999999289, 0.000000000000000000 ) ) ;
#9550 = AXIS2_PLACEMENT_3D ( 'NONE', #2428, #819, #2475 ) ;
#9551 = DIRECTION ( 'NONE',  ( 0.7849198975831888081, 0.000000000000000000, -0.6195972517514876099 ) ) ;
#9552 = AXIS2_PLACEMENT_3D ( 'NONE', #6515, #8100, #7364 ) ;
#9553 = AXIS2_PLACEMENT_3D ( 'NONE', #315, #6325, #5548 ) ;
#9554 = ORIENTED_EDGE ( 'NONE', *, *, #4513, .F. ) ;
#9555 = DIRECTION ( 'NONE',  ( 0.000000000000000000, 0.000000000000000000, -1.000000000000000000 ) ) ;
#9556 = CONICAL_SURFACE ( 'NONE', #1508, 1.610000000000000098, 0.7853981633974463916 ) ;
#9557 = ORIENTED_EDGE ( 'NONE', *, *, #7086, .F. ) ;
#9558 = CYLINDRICAL_SURFACE ( 'NONE', #3286, 38.00000000000000000 ) ;
#9559 = DIRECTION ( 'NONE',  ( 0.000000000000000000, -1.000000000000000000, 0.000000000000000000 ) ) ;
#9560 = CARTESIAN_POINT ( 'NONE',  ( 11.41459187292171151, 11.09818508355548872, 37.29611385600085072 ) ) ;
#9561 = DIRECTION ( 'NONE',  ( 1.735493991486224571E-29, 0.000000000000000000, -1.000000000000000000 ) ) ;
#9562 = EDGE_CURVE ( 'NONE', #9184, #7653, #5326, .T. ) ;
#9563 = DIRECTION ( 'NONE',  ( -0.6195972517514876099, 0.000000000000000000, -0.7849198975831889191 ) ) ;
#9564 = AXIS2_PLACEMENT_3D ( 'NONE', #7691, #7077, #5102 ) ;
#9565 = EDGE_CURVE ( 'NONE', #7120, #6350, #5624, .T. ) ;
#9566 = EDGE_CURVE ( 'NONE', #3257, #2396, #4540, .T. ) ;
#9567 = DIRECTION ( 'NONE',  ( -1.000000000000000000, -0.000000000000000000, -0.000000000000000000 ) ) ;
#9568 = LINE ( 'NONE', #6679, #9155 ) ;
#9569 = AXIS2_PLACEMENT_3D ( 'NONE', #7157, #1143, #4164 ) ;
#9570 = ORIENTED_EDGE ( 'NONE', *, *, #5945, .F. ) ;
#9571 = FACE_OUTER_BOUND ( 'NONE', #6714, .T. ) ;
#9572 = CARTESIAN_POINT ( 'NONE',  ( 9.671127104547153408, 5.921967959015561611, 41.54032951960448372 ) ) ;
#9573 = EDGE_CURVE ( 'NONE', #2848, #2873, #125, .T. ) ;
#9574 = VERTEX_POINT ( 'NONE', #5904 ) ;
#9575 = DIRECTION ( 'NONE',  ( 1.735493991486225972E-29, -6.508102468073347395E-30, -1.000000000000000000 ) ) ;
#9576 = PLANE ( 'NONE',  #3901 ) ;
#9577 = CARTESIAN_POINT ( 'NONE',  ( -12.23816054246644036, -2.710493630309420254, 37.03212527134820675 ) ) ;
#9578 = CARTESIAN_POINT ( 'NONE',  ( -5.562309845534584518, 49.99999999999999289, 33.06426808735054124 ) ) ;
#9579 = ADVANCED_FACE ( 'NONE', ( #3688 ), #6836, .F. ) ;
#9580 = ADVANCED_FACE ( 'NONE', ( #5269 ), #8230, .T. ) ;
#9581 = EDGE_CURVE ( 'NONE', #5230, #4753, #4377, .T. ) ;
#9582 = EDGE_CURVE ( 'NONE', #8853, #9115, #6042, .T. ) ;
#9583 = FACE_OUTER_BOUND ( 'NONE', #5061, .T. ) ;
#9584 = ORIENTED_EDGE ( 'NONE', *, *, #2728, .T. ) ;
#9585 = DIRECTION ( 'NONE',  ( 0.000000000000000000, 1.000000000000000000, 0.000000000000000000 ) ) ;
#9586 = CARTESIAN_POINT ( 'NONE',  ( -0.1907661894286938054, -15.00000000000000000, 30.58171691558911931 ) ) ;
#9587 = VERTEX_POINT ( 'NONE', #8932 ) ;
#9588 = LINE ( 'NONE', #602, #9498 ) ;
#9589 = DIRECTION ( 'NONE',  ( 0.000000000000000000, 0.000000000000000000, -1.000000000000000000 ) ) ;
#9590 = CARTESIAN_POINT ( 'NONE',  ( 7.315962409250510667, 10.12005692215709196, 42.61102608560413785 ) ) ;
#9591 = DIRECTION ( 'NONE',  ( 0.000000000000000000, -1.000000000000000000, 0.000000000000000000 ) ) ;
#9592 = ORIENTED_EDGE ( 'NONE', *, *, #4770, .T. ) ;
#9593 = CARTESIAN_POINT ( 'NONE',  ( -34.72826512091049267, 59.61718548957851027, -3.689690490709783166 ) ) ;
#9594 = DIRECTION ( 'NONE',  ( -0.000000000000000000, -0.000000000000000000, 1.000000000000000000 ) ) ;
#9595 = ORIENTED_EDGE ( 'NONE', *, *, #7697, .T. ) ;
#9596 = FACE_OUTER_BOUND ( 'NONE', #7557, .T. ) ;
#9597 = EDGE_LOOP ( 'NONE', ( #568, #5377 ) ) ;
#9598 = CARTESIAN_POINT ( 'NONE',  ( -8.358540341008785290, 8.859167319972213406, 38.23848664195695335 ) ) ;
#9599 = CARTESIAN_POINT ( 'NONE',  ( 12.20000000000000107, 0.000000000000000000, 0.000000000000000000 ) ) ;
#9600 = CARTESIAN_POINT ( 'NONE',  ( 3.885274725274726393, -8.673617379884035472E-16, 0.000000000000000000 ) ) ;
#9601 = B_SPLINE_CURVE_WITH_KNOTS ( 'NONE', 3,
 ( #4012, #271, #3260, #2508 ),
 .UNSPECIFIED., .F., .F.,
 ( 4, 4 ),
 ( 0.000000000000000000, 0.003679109433542032855 ),
 .UNSPECIFIED. ) ;
#9602 = ORIENTED_EDGE ( 'NONE', *, *, #9217, .T. ) ;
#9603 = CARTESIAN_POINT ( 'NONE',  ( -5.562309845534701758, 61.99999999999999289, 33.06426808735052703 ) ) ;
#9604 = ORIENTED_EDGE ( 'NONE', *, *, #1305, .F. ) ;
#9605 = DIRECTION ( 'NONE',  ( -0.7071067811865489050, 8.659560562354915602E-17, -0.7071067811865462405 ) ) ;
#9606 = DIRECTION ( 'NONE',  ( -1.735493991486225972E-29, 6.508102468073347395E-30, 1.000000000000000000 ) ) ;
#9607 = FACE_BOUND ( 'NONE', #8707, .T. ) ;
#9608 = DIRECTION ( 'NONE',  ( 0.000000000000000000, 0.000000000000000000, 1.000000000000000000 ) ) ;
#9609 = EDGE_CURVE ( 'NONE', #7854, #8367, #8057, .T. ) ;
#9610 = DIRECTION ( 'NONE',  ( 0.000000000000000000, 0.000000000000000000, -1.000000000000000000 ) ) ;
#9611 = VERTEX_POINT ( 'NONE', #2942 ) ;
#9612 = CARTESIAN_POINT ( 'NONE',  ( 7.742466688136331219E-27, 42.50000000000020606, 2.935117235246147440E-28 ) ) ;
#9613 = CARTESIAN_POINT ( 'NONE',  ( 1.342554273002455556, 13.20990960304843931, 43.95670083747006629 ) ) ;
#9614 = VERTEX_POINT ( 'NONE', #8187 ) ;
#9615 = FACE_OUTER_BOUND ( 'NONE', #7820, .T. ) ;
#9616 = CARTESIAN_POINT ( 'NONE',  ( 8.283039504820623957E-27, 44.50000000000019185, -24.09806918451535651 ) ) ;
#9617 = CIRCLE ( 'NONE', #8680, 31.50000000000000000 ) ;
#9618 = AXIS2_PLACEMENT_3D ( 'NONE', #1710, #2393, #4727 ) ;
#9619 = CARTESIAN_POINT ( 'NONE',  ( -6.000000000000005329, -15.00000000000000000, -26.32489316217636954 ) ) ;
#9620 = VECTOR ( 'NONE', #3533, 1000.000000000000000 ) ;
#9621 = CYLINDRICAL_SURFACE ( 'NONE', #3865, 31.50000000000000000 ) ;
#9622 = VERTEX_POINT ( 'NONE', #3034 ) ;
#9623 = CARTESIAN_POINT ( 'NONE',  ( -4.904043666719616112, 60.99999999999999289, -31.11591804390330651 ) ) ;
#9624 = CARTESIAN_POINT ( 'NONE',  ( -10.67413343474082588, -5.256176925685571710, 37.51319708726573765 ) ) ;
#9625 = ORIENTED_EDGE ( 'NONE', *, *, #7146, .T. ) ;
#9626 = ADVANCED_FACE ( 'NONE', ( #8335 ), #4436, .F. ) ;
#9627 = ADVANCED_FACE ( 'NONE', ( #8282 ), #43, .T. ) ;
#9628 = AXIS2_PLACEMENT_3D ( 'NONE', #3677, #3731, #9561 ) ;
#9629 = EDGE_CURVE ( 'NONE', #8756, #1203, #2323, .T. ) ;
#9630 = LINE ( 'NONE', #7307, #8553 ) ;
#9631 = DIRECTION ( 'NONE',  ( -0.000000000000000000, 1.000000000000000000, -0.000000000000000000 ) ) ;
#9632 = CARTESIAN_POINT ( 'NONE',  ( 0.8980271448007615120, 18.26880201182753538, 38.99211230656880645 ) ) ;
#9633 = ITEM_DEFINED_TRANSFORMATION ( 'NONE', 'NONE', #347,  #6314 ) ;
#9634 = AXIS2_PLACEMENT_3D ( 'NONE', #9315, #8577, #3988 ) ;
#9635 = VERTEX_POINT ( 'NONE', #779 ) ;
#9636 = DIRECTION ( 'NONE',  ( 0.000000000000000000, 1.000000000000000000, 0.000000000000000000 ) ) ;
#9637 = ORIENTED_EDGE ( 'NONE', *, *, #273, .T. ) ;
#9638 = CARTESIAN_POINT ( 'NONE',  ( 33.06426808735054124, 59.99576382555915899, 3.062309845534584074 ) ) ;
#9639 = VERTEX_POINT ( 'NONE', #4484 ) ;
#9640 = LINE ( 'NONE', #4411, #7190 ) ;
#9641 = ORIENTED_EDGE ( 'NONE', *, *, #9311, .F. ) ;
#9642 = CARTESIAN_POINT ( 'NONE',  ( -6.647844517998846570, 16.29448827485380136, 38.43121571274925685 ) ) ;
#9643 = DIRECTION ( 'NONE',  ( 0.000000000000000000, -1.000000000000000000, 0.000000000000000000 ) ) ;
#9644 = AXIS2_PLACEMENT_3D ( 'NONE', #6930, #5559, #190 ) ;
#9645 = AXIS2_PLACEMENT_3D ( 'NONE', #4365, #508, #421 ) ;
#9646 = DIRECTION ( 'NONE',  ( -0.9860132971832693549, -1.788557213313974126E-28, 0.1666666666666657970 ) ) ;
#9647 = MANIFOLD_SOLID_BREP ( 'Chamfer2', #6088 ) ;
#9648 = CIRCLE ( 'NONE', #977, 38.00000000000000000 ) ;
#9649 = EDGE_LOOP ( 'NONE', ( #6206, #1703, #765, #9439, #36, #277 ) ) ;
#9650 = CARTESIAN_POINT ( 'NONE',  ( -5.666666666666482222, 19.33333333333320780, 19.33333333333351334 ) ) ;
#9651 = ORIENTED_EDGE ( 'NONE', *, *, #1386, .T. ) ;
#9652 = CARTESIAN_POINT ( 'NONE',  ( 0.000000000000000000, 39.99999999999999289, 0.000000000000000000 ) ) ;
#9653 = DIRECTION ( 'NONE',  ( 1.735493991486225972E-29, -6.508102468073347395E-30, -1.000000000000000000 ) ) ;
#9654 = CARTESIAN_POINT ( 'NONE',  ( 0.000000000000000000, 0.000000000000000000, 0.000000000000000000 ) ) ;
#9655 = CARTESIAN_POINT ( 'NONE',  ( 5.562309845534588959, 59.99999999999999289, -33.06426808735054124 ) ) ;
#9656 = AXIS2_PLACEMENT_3D ( 'NONE', #3766, #6914, #6128 ) ;
#9657 = FILL_AREA_STYLE_COLOUR ( '', #4191 ) ;
#9658 = ADVANCED_FACE ( 'NONE', ( #9274 ), #9027, .F. ) ;
#9659 = DIRECTION ( 'NONE',  ( -0.000000000000000000, -1.000000000000000000, -0.000000000000000000 ) ) ;
#9660 = ORIENTED_EDGE ( 'NONE', *, *, #4328, .T. ) ;
#9661 = CARTESIAN_POINT ( 'NONE',  ( 1.040310318760209318E-26, 50.00000000000032685, -25.00000000000000000 ) ) ;
#9662 = CARTESIAN_POINT ( 'NONE',  ( 0.000000000000000000, 38.99999999999993605, 0.000000000000000000 ) ) ;
#9663 = DIRECTION ( 'NONE',  ( -1.820952055660014662E-28, -1.000000000000000000, -7.038118388768679669E-30 ) ) ;
#9664 = CARTESIAN_POINT ( 'NONE',  ( 6.848559158202236041, -15.00000000000000178, 28.25275382344465314 ) ) ;
#9665 = DIRECTION ( 'NONE',  ( -0.9449569463147374782, 0.000000000000000000, -0.3271946967961528729 ) ) ;
#9666 = DIRECTION ( 'NONE',  ( 0.000000000000000000, 0.000000000000000000, 1.000000000000000000 ) ) ;
#9667 = CIRCLE ( 'NONE', #61, 25.00000000000000000 ) ;
#9668 = CIRCLE ( 'NONE', #1159, 4.500000000000005329 ) ;
#9669 = DIRECTION ( 'NONE',  ( -0.9860132971832694659, -1.788557213313974350E-28, 0.1666666666666658247 ) ) ;
#9670 = DIRECTION ( 'NONE',  ( 0.000000000000000000, 0.000000000000000000, 1.000000000000000000 ) ) ;
#9671 = ORIENTED_EDGE ( 'NONE', *, *, #7093, .T. ) ;
#9672 = CARTESIAN_POINT ( 'NONE',  ( 1.084683744678891232E-26, 53.00000000000031974, -25.00000000000000000 ) ) ;
#9673 = CARTESIAN_POINT ( 'NONE',  ( 0.5290539970386457513, -9.461942445008636682, 39.52372684969373040 ) ) ;
#9674 = ORIENTED_EDGE ( 'NONE', *, *, #6525, .T. ) ;
#9675 = CARTESIAN_POINT ( 'NONE',  ( -5.562309845534701758, 61.83753588906734677, 37.56426808735052703 ) ) ;
#9676 = LINE ( 'NONE', #3560, #102 ) ;
#9677 = EDGE_LOOP ( 'NONE', ( #6111, #5489, #3805, #8323 ) ) ;
#9678 = CARTESIAN_POINT ( 'NONE',  ( 12.61936450812443056, 8.119135588597398367, 36.90359936746606451 ) ) ;
#9679 = ADVANCED_FACE ( 'NONE', ( #3133 ), #3233, .T. ) ;
#9680 = DIRECTION ( 'NONE',  ( 0.000000000000000000, 0.000000000000000000, 1.000000000000000000 ) ) ;
#9681 = VECTOR ( 'NONE', #328, 1000.000000000000000 ) ;
#9682 = ORIENTED_EDGE ( 'NONE', *, *, #1375, .T. ) ;
#9683 = CARTESIAN_POINT ( 'NONE',  ( -35.23154690738756756, 59.33548969180893806, -4.305939634252483827 ) ) ;
#9684 = ADVANCED_FACE ( 'NONE', ( #5477 ), #1618, .T. ) ;
#9685 = ORIENTED_EDGE ( 'NONE', *, *, #8776, .T. ) ;
#9686 = CARTESIAN_POINT ( 'NONE',  ( 35.56433427405016090, 59.02194934605864063, 5.394111410765026093 ) ) ;
#9687 = VERTEX_POINT ( 'NONE', #9179 ) ;
#9688 = DIRECTION ( 'NONE',  ( -0.000000000000000000, -1.000000000000000000, -0.000000000000000000 ) ) ;
#9689 = ADVANCED_FACE ( 'NONE', ( #4641 ), #7693, .T. ) ;
#9690 = CIRCLE ( 'NONE', #7801, 25.00000000000000000 ) ;
#9691 = ORIENTED_EDGE ( 'NONE', *, *, #2372, .F. ) ;
#9692 = CARTESIAN_POINT ( 'NONE',  ( -3.453443797567174123, 17.81395218307918427, 38.85641742718816261 ) ) ;
#9693 = CARTESIAN_POINT ( 'NONE',  ( 26.32489316217636954, -15.00000000000000000, -6.000000000000006217 ) ) ;
#9694 = CARTESIAN_POINT ( 'NONE',  ( 0.000000000000000000, 54.99999999999999289, 0.000000000000000000 ) ) ;
#9695 = TOROIDAL_SURFACE ( 'NONE', #3211, 33.00000000000000711, 5.000000000000000000 ) ;
#9696 = MANIFOLD_SOLID_BREP ( 'Hex', #8627 ) ;
#9697 = AXIS2_PLACEMENT_3D ( 'NONE', #3551, #6560, #8741 ) ;
#9698 = EDGE_CURVE ( 'NONE', #7616, #3887, #9174, .T. ) ;
#9699 = ORIENTED_EDGE ( 'NONE', *, *, #2945, .T. ) ;
#9700 = DIRECTION ( 'NONE',  ( 0.000000000000000000, 0.000000000000000000, 1.000000000000000000 ) ) ;
#9701 = EDGE_CURVE ( 'NONE', #3761, #2408, #7035, .T. ) ;
#9702 = ORIENTED_EDGE ( 'NONE', *, *, #3287, .F. ) ;
#9703 = VECTOR ( 'NONE', #4944, 1000.000000000000000 ) ;
#9704 = EDGE_CURVE ( 'NONE', #8597, #7666, #7389, .T. ) ;
#9705 = CARTESIAN_POINT ( 'NONE',  ( -29.00000000000000355, 0.000000000000000000, 4.000000000000010658 ) ) ;
#9706 = VECTOR ( 'NONE', #6984, 1000.000000000000000 ) ;
#9707 = CARTESIAN_POINT ( 'NONE',  ( 0.000000000000000000, 30.00000000000000000, 0.000000000000000000 ) ) ;
#9708 = DIRECTION ( 'NONE',  ( 1.820952055660014662E-28, 1.000000000000000000, -6.508102468073347395E-30 ) ) ;
#9709 = CIRCLE ( 'NONE', #4351, 33.00000000000000711 ) ;
#9710 = AXIS2_PLACEMENT_3D ( 'NONE', #8227, #1371, #4482 ) ;
#9711 = AXIS2_PLACEMENT_3D ( 'NONE', #8875, #3683, #2985 ) ;
#9712 = AXIS2_PLACEMENT_3D ( 'NONE', #5839, #2030, #5884 ) ;
#9713 = CARTESIAN_POINT ( 'NONE',  ( -5.562309845534584518, 59.99999999999999289, 33.06426808735054124 ) ) ;
#9714 = VERTEX_POINT ( 'NONE', #8634 ) ;
#9715 = DIRECTION ( 'NONE',  ( 0.000000000000000000, 0.000000000000000000, 1.000000000000000000 ) ) ;
#9716 = DIRECTION ( 'NONE',  ( -0.000000000000000000, 1.000000000000000000, -0.000000000000000000 ) ) ;
#9717 = CARTESIAN_POINT ( 'NONE',  ( 0.000000000000000000, 1.000000000000014655, 0.000000000000000000 ) ) ;
#9718 = B_SPLINE_CURVE_WITH_KNOTS ( 'NONE', 3,
 ( #7532, #764, #2375, #864 ),
 .UNSPECIFIED., .F., .F.,
 ( 4, 4 ),
 ( 0.009125339089286726990, 0.009329711147074801203 ),
 .UNSPECIFIED. ) ;
#9719 = AXIS2_PLACEMENT_3D ( 'NONE', #70, #9053, #3010 ) ;
#9720 = DIRECTION ( 'NONE',  ( 0.000000000000000000, 1.000000000000000000, 0.000000000000000000 ) ) ;
#9721 = CARTESIAN_POINT ( 'NONE',  ( 29.24912810952613640, 29.14236109046821710, -6.000000000000006217 ) ) ;
#9722 = CARTESIAN_POINT ( 'NONE',  ( -6.150308060456896264, 16.61224636055649384, 38.51628361999085115 ) ) ;
#9723 = ADVANCED_FACE ( 'NONE', ( #4329 ), #5019, .T. ) ;
#9724 = CIRCLE ( 'NONE', #6871, 3.000000000000002665 ) ;
#9725 = DIRECTION ( 'NONE',  ( -1.000000000000000000, -0.000000000000000000, -0.000000000000000000 ) ) ;
#9726 = ORIENTED_EDGE ( 'NONE', *, *, #3649, .T. ) ;
#9727 = CARTESIAN_POINT ( 'NONE',  ( -8.216777476527294510, 54.50000000000031264, -23.61111111111111427 ) ) ;
#9728 = CARTESIAN_POINT ( 'NONE',  ( 11.07761026121385584, -15.00000000000000000, 37.39366993089404900 ) ) ;
#9729 = ORIENTED_EDGE ( 'NONE', *, *, #3351, .T. ) ;
#9730 = CARTESIAN_POINT ( 'NONE',  ( 0.000000000000000000, -15.00000000000000000, 0.000000000000000000 ) ) ;
#9731 = CIRCLE ( 'NONE', #9265, 26.00000000000017408 ) ;
#9732 = FACE_OUTER_BOUND ( 'NONE', #4757, .T. ) ;
#9733 = ORIENTED_EDGE ( 'NONE', *, *, #760, .F. ) ;
#9734 = CARTESIAN_POINT ( 'NONE',  ( 7.039660980758952746, -3.873581541912419546, 38.48359011748724612 ) ) ;
#9735 = PRODUCT_CONTEXT ( 'NONE', #3089, 'mechanical' ) ;
#9736 = ADVANCED_FACE ( 'NONE', ( #4186, #7335 ), #6486, .T. ) ;
#9737 = ORIENTED_EDGE ( 'NONE', *, *, #1249, .T. ) ;
#9738 = CARTESIAN_POINT ( 'NONE',  ( 33.06426808735054124, 59.99999999999999289, 5.562309845534586294 ) ) ;
#9739 = CARTESIAN_POINT ( 'NONE',  ( 5.562309845534588959, 49.99999999999999289, -35.56426808735054834 ) ) ;
#9740 = VERTEX_POINT ( 'NONE', #1120 ) ;
#9741 = DIRECTION ( 'NONE',  ( -0.000000000000000000, -1.000000000000000000, -0.000000000000000000 ) ) ;
#9742 = VERTEX_POINT ( 'NONE', #4138 ) ;
#9743 = CARTESIAN_POINT ( 'NONE',  ( -4.444672669478428872, 12.25879546470133974, 43.49417769924191646 ) ) ;
#9744 = EDGE_CURVE ( 'NONE', #874, #1345, #8817, .T. ) ;
#9745 = DIRECTION ( 'NONE',  ( 0.000000000000000000, 0.000000000000000000, -1.000000000000000000 ) ) ;
#9746 = ADVANCED_FACE ( 'NONE', ( #383 ), #9468, .F. ) ;
#9747 = DIRECTION ( 'NONE',  ( 0.000000000000000000, 0.000000000000000000, -1.000000000000000000 ) ) ;
#9748 = ADVANCED_BREP_SHAPE_REPRESENTATION ( '', ( #6323, #6314 ), #2196 ) ;
#9749 = EDGE_LOOP ( 'NONE', ( #716, #3550, #8181, #5930, #5046 ) ) ;
#9750 = CARTESIAN_POINT ( 'NONE',  ( -7.740900945811527656, -7.145159734021766518, 38.44003917021594674 ) ) ;
#9751 = CARTESIAN_POINT ( 'NONE',  ( 6.000000000000001776, 27.42469319230600533, -31.00000000000000711 ) ) ;
#9752 = CARTESIAN_POINT ( 'NONE',  ( 1.300000000000000044, 3.252606517456513302E-16, 2.499999999999999556 ) ) ;
#9753 = CARTESIAN_POINT ( 'NONE',  ( -8.216777476527294510, 45.50000000000019185, -23.61111111111111427 ) ) ;
#9754 = NEXT_ASSEMBLY_USAGE_OCCURRENCE ( 'NAUO1', ' ', ' ', #4948, #8147, $ ) ;
#9755 = NEXT_ASSEMBLY_USAGE_OCCURRENCE ( 'NAUO2', ' ', ' ', #4948, #1863, $ ) ;
#9756 = NEXT_ASSEMBLY_USAGE_OCCURRENCE ( 'NAUO3', ' ', ' ', #4948, #8871, $ ) ;
#9757 = NEXT_ASSEMBLY_USAGE_OCCURRENCE ( 'NAUO4', ' ', ' ', #4948, #850, $ ) ;
#9758 = NEXT_ASSEMBLY_USAGE_OCCURRENCE ( 'NAUO5', ' ', ' ', #4948, #8871, $ ) ;
#9759 = NEXT_ASSEMBLY_USAGE_OCCURRENCE ( 'NAUO6', ' ', ' ', #4948, #8871, $ ) ;
#9760 = NEXT_ASSEMBLY_USAGE_OCCURRENCE ( 'NAUO7', ' ', ' ', #4948, #8871, $ ) ;
#9761 = NEXT_ASSEMBLY_USAGE_OCCURRENCE ( 'NAUO8', ' ', ' ', #4948, #436, $ ) ;
#9762 = NEXT_ASSEMBLY_USAGE_OCCURRENCE ( 'NAUO9', ' ', ' ', #4948, #436, $ ) ;
#9763 = NEXT_ASSEMBLY_USAGE_OCCURRENCE ( 'NAUO10', ' ', ' ', #4948, #436, $ ) ;
#9764 = NEXT_ASSEMBLY_USAGE_OCCURRENCE ( 'NAUO11', ' ', ' ', #4948, #436, $ ) ;
#9765=COLOUR_RGB('Dark Blue',0.08,0.2,0.34);
#9766=FILL_AREA_STYLE_COLOUR('',#9765);
#9767=FILL_AREA_STYLE('',(#9766));
#9768=SURFACE_STYLE_FILL_AREA(#9767);
#9769=SURFACE_SIDE_STYLE('',(#9768));
#9770=SURFACE_STYLE_USAGE(.BOTH.,#9769);
#9771=PRESENTATION_STYLE_ASSIGNMENT((#9770));
#9772=COLOUR_RGB('Light Blue',0.38,0.62,0.78);
#9773=FILL_AREA_STYLE_COLOUR('',#9772);
#9774=FILL_AREA_STYLE('',(#9773));
#9775=SURFACE_STYLE_FILL_AREA(#9774);
#9776=SURFACE_SIDE_STYLE('',(#9775));
#9777=SURFACE_STYLE_USAGE(.BOTH.,#9776);
#9778=PRESENTATION_STYLE_ASSIGNMENT((#9777));
#9779=COLOUR_RGB('Sky Blue',0.24,0.69,0.87);
#9780=FILL_AREA_STYLE_COLOUR('',#9779);
#9781=FILL_AREA_STYLE('',(#9780));
#9782=SURFACE_STYLE_FILL_AREA(#9781);
#9783=SURFACE_SIDE_STYLE('',(#9782));
#9784=SURFACE_STYLE_USAGE(.BOTH.,#9783);
#9785=PRESENTATION_STYLE_ASSIGNMENT((#9784));
#9786=COLOUR_RGB('Grey',0.48,0.52,0.57);
#9787=FILL_AREA_STYLE_COLOUR('',#9786);
#9788=FILL_AREA_STYLE('',(#9787));
#9789=SURFACE_STYLE_FILL_AREA(#9788);
#9790=SURFACE_SIDE_STYLE('',(#9789));
#9791=SURFACE_STYLE_USAGE(.BOTH.,#9790);
#9792=PRESENTATION_STYLE_ASSIGNMENT((#9791));
#9793=COLOUR_RGB('Black',0.12,0.14,0.17);
#9794=FILL_AREA_STYLE_COLOUR('',#9793);
#9795=FILL_AREA_STYLE('',(#9794));
#9796=SURFACE_STYLE_FILL_AREA(#9795);
#9797=SURFACE_SIDE_STYLE('',(#9796));
#9798=SURFACE_STYLE_USAGE(.BOTH.,#9797);
#9799=PRESENTATION_STYLE_ASSIGNMENT((#9798));
#9800=COLOUR_RGB('Off White',0.89,0.88,0.83);
#9801=FILL_AREA_STYLE_COLOUR('',#9800);
#9802=FILL_AREA_STYLE('',(#9801));
#9803=SURFACE_STYLE_FILL_AREA(#9802);
#9804=SURFACE_SIDE_STYLE('',(#9803));
#9805=SURFACE_STYLE_USAGE(.BOTH.,#9804);
#9806=PRESENTATION_STYLE_ASSIGNMENT((#9805));
ENDSEC;
END-ISO-10303-21;
